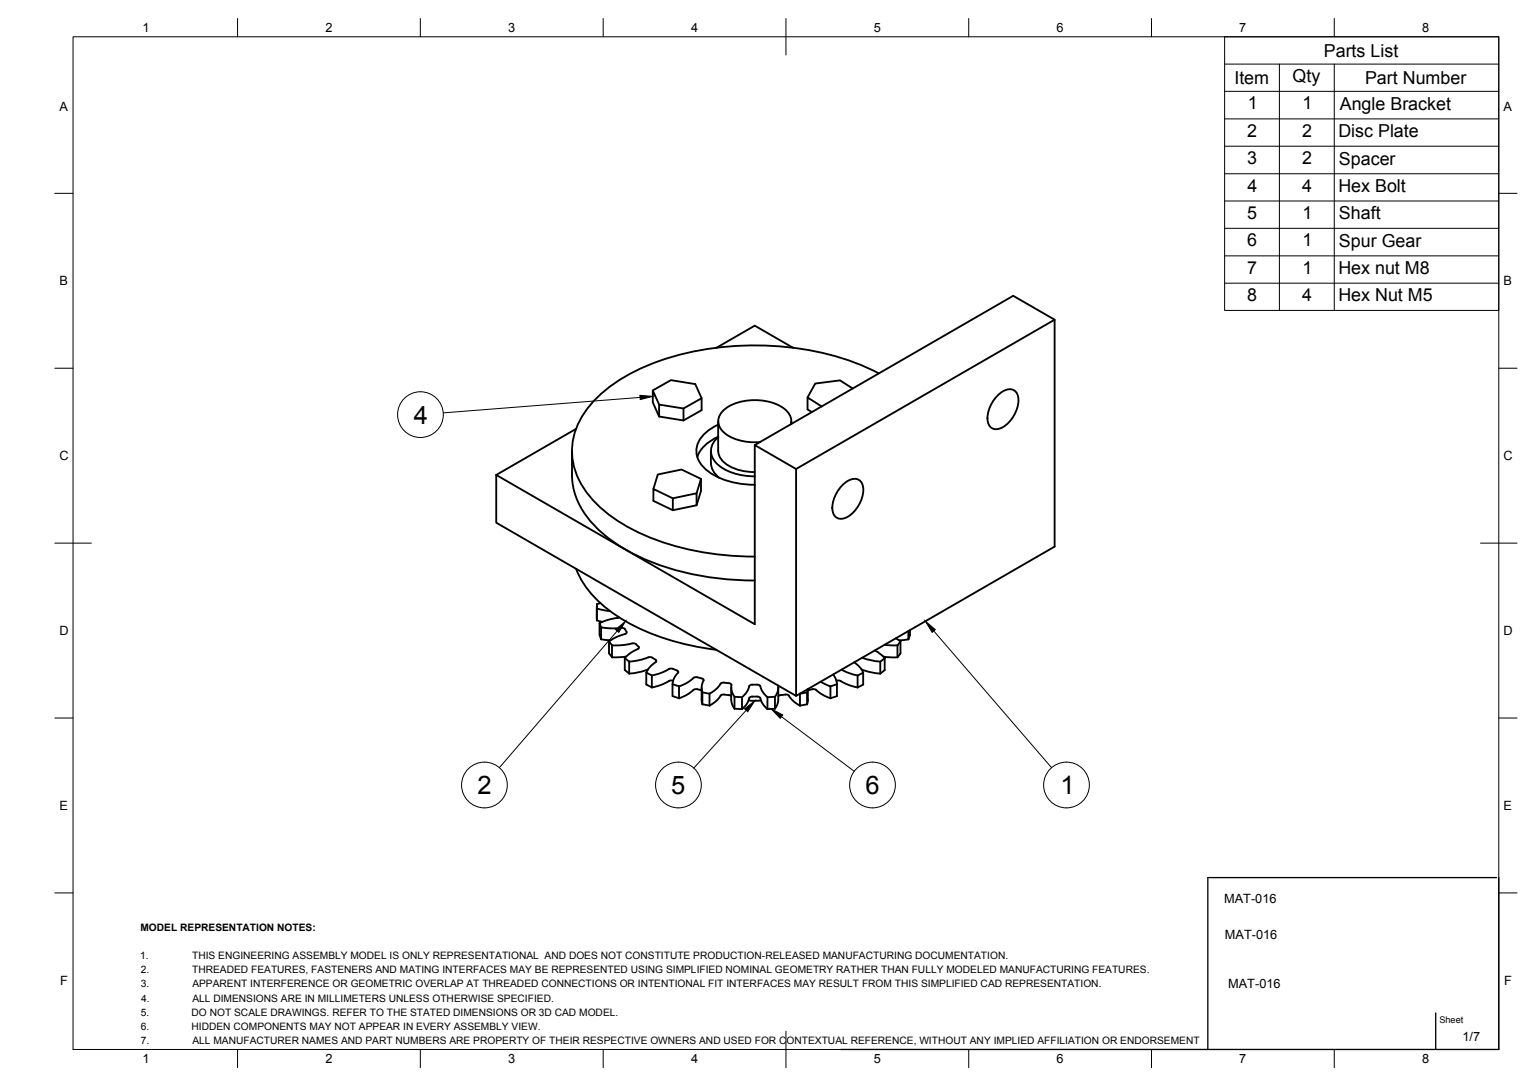
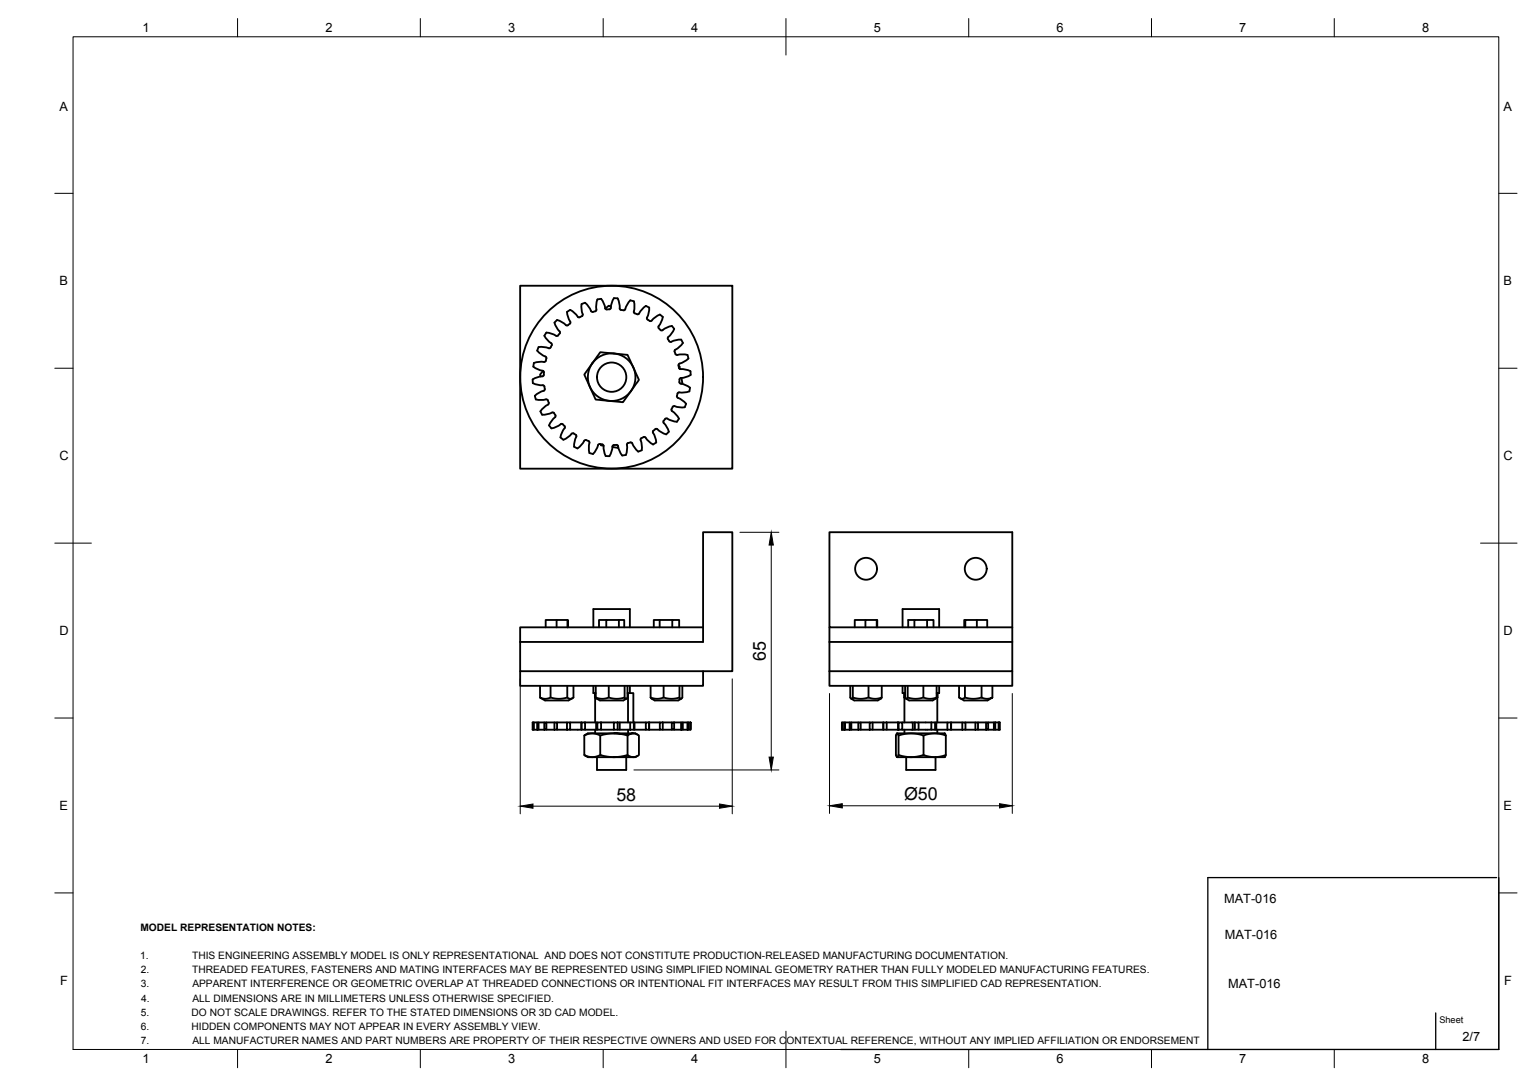
ISO-10303-21;
HEADER;
/* Generated by software containing ST-Developer
 * from STEP Tools, Inc. (www.steptools.com) 
 */

FILE_DESCRIPTION(
/* description */ ('STEP AP214'),
/* implementation_level */ '2;1');

FILE_NAME(
/* name */ 'MAT-016.step',
/* time_stamp */ '2026-11-14T06:10:26-08:00',
/* author */ (''),
/* organization */ (''),
/* preprocessor_version */ 'ST-DEVELOPER v20.2',
/* originating_system */ 'Autodesk Translation Framework v15.17.0.0',
/* authorisation */ '');

FILE_SCHEMA (('AUTOMOTIVE_DESIGN { 1 0 10303 214 3 1 1 }'));
ENDSEC;

DATA;
#10=MECHANICAL_DESIGN_GEOMETRIC_PRESENTATION_REPRESENTATION('',(#164,#165,
#166,#167,#168,#169,#170,#171),#10413);
#11=ITEM_DEFINED_TRANSFORMATION($,$,#5397,#6134);
#12=ITEM_DEFINED_TRANSFORMATION($,$,#6051,#6135);
#13=ITEM_DEFINED_TRANSFORMATION($,$,#6076,#6136);
#14=ITEM_DEFINED_TRANSFORMATION($,$,#6085,#6137);
#15=ITEM_DEFINED_TRANSFORMATION($,$,#5435,#6138);
#16=ITEM_DEFINED_TRANSFORMATION($,$,#5466,#6139);
#17=ITEM_DEFINED_TRANSFORMATION($,$,#6015,#6140);
#18=ITEM_DEFINED_TRANSFORMATION($,$,#6098,#6141);
#19=ITEM_DEFINED_TRANSFORMATION($,$,#6051,#6142);
#20=ITEM_DEFINED_TRANSFORMATION($,$,#6076,#6143);
#21=ITEM_DEFINED_TRANSFORMATION($,$,#6085,#6144);
#22=ITEM_DEFINED_TRANSFORMATION($,$,#6085,#6145);
#23=ITEM_DEFINED_TRANSFORMATION($,$,#6085,#6146);
#24=ITEM_DEFINED_TRANSFORMATION($,$,#6098,#6147);
#25=ITEM_DEFINED_TRANSFORMATION($,$,#6098,#6148);
#26=ITEM_DEFINED_TRANSFORMATION($,$,#6098,#6149);
#27=(
REPRESENTATION_RELATIONSHIP($,$,#10453,#10452)
REPRESENTATION_RELATIONSHIP_WITH_TRANSFORMATION(#11)
SHAPE_REPRESENTATION_RELATIONSHIP()
);
#28=(
REPRESENTATION_RELATIONSHIP($,$,#10457,#10452)
REPRESENTATION_RELATIONSHIP_WITH_TRANSFORMATION(#12)
SHAPE_REPRESENTATION_RELATIONSHIP()
);
#29=(
REPRESENTATION_RELATIONSHIP($,$,#10458,#10452)
REPRESENTATION_RELATIONSHIP_WITH_TRANSFORMATION(#13)
SHAPE_REPRESENTATION_RELATIONSHIP()
);
#30=(
REPRESENTATION_RELATIONSHIP($,$,#10459,#10452)
REPRESENTATION_RELATIONSHIP_WITH_TRANSFORMATION(#14)
SHAPE_REPRESENTATION_RELATIONSHIP()
);
#31=(
REPRESENTATION_RELATIONSHIP($,$,#10454,#10452)
REPRESENTATION_RELATIONSHIP_WITH_TRANSFORMATION(#15)
SHAPE_REPRESENTATION_RELATIONSHIP()
);
#32=(
REPRESENTATION_RELATIONSHIP($,$,#10455,#10452)
REPRESENTATION_RELATIONSHIP_WITH_TRANSFORMATION(#16)
SHAPE_REPRESENTATION_RELATIONSHIP()
);
#33=(
REPRESENTATION_RELATIONSHIP($,$,#10456,#10452)
REPRESENTATION_RELATIONSHIP_WITH_TRANSFORMATION(#17)
SHAPE_REPRESENTATION_RELATIONSHIP()
);
#34=(
REPRESENTATION_RELATIONSHIP($,$,#10460,#10452)
REPRESENTATION_RELATIONSHIP_WITH_TRANSFORMATION(#18)
SHAPE_REPRESENTATION_RELATIONSHIP()
);
#35=(
REPRESENTATION_RELATIONSHIP($,$,#10457,#10452)
REPRESENTATION_RELATIONSHIP_WITH_TRANSFORMATION(#19)
SHAPE_REPRESENTATION_RELATIONSHIP()
);
#36=(
REPRESENTATION_RELATIONSHIP($,$,#10458,#10452)
REPRESENTATION_RELATIONSHIP_WITH_TRANSFORMATION(#20)
SHAPE_REPRESENTATION_RELATIONSHIP()
);
#37=(
REPRESENTATION_RELATIONSHIP($,$,#10459,#10452)
REPRESENTATION_RELATIONSHIP_WITH_TRANSFORMATION(#21)
SHAPE_REPRESENTATION_RELATIONSHIP()
);
#38=(
REPRESENTATION_RELATIONSHIP($,$,#10459,#10452)
REPRESENTATION_RELATIONSHIP_WITH_TRANSFORMATION(#22)
SHAPE_REPRESENTATION_RELATIONSHIP()
);
#39=(
REPRESENTATION_RELATIONSHIP($,$,#10459,#10452)
REPRESENTATION_RELATIONSHIP_WITH_TRANSFORMATION(#23)
SHAPE_REPRESENTATION_RELATIONSHIP()
);
#40=(
REPRESENTATION_RELATIONSHIP($,$,#10460,#10452)
REPRESENTATION_RELATIONSHIP_WITH_TRANSFORMATION(#24)
SHAPE_REPRESENTATION_RELATIONSHIP()
);
#41=(
REPRESENTATION_RELATIONSHIP($,$,#10460,#10452)
REPRESENTATION_RELATIONSHIP_WITH_TRANSFORMATION(#25)
SHAPE_REPRESENTATION_RELATIONSHIP()
);
#42=(
REPRESENTATION_RELATIONSHIP($,$,#10460,#10452)
REPRESENTATION_RELATIONSHIP_WITH_TRANSFORMATION(#26)
SHAPE_REPRESENTATION_RELATIONSHIP()
);
#43=CONTEXT_DEPENDENT_SHAPE_REPRESENTATION(#27,#10436);
#44=CONTEXT_DEPENDENT_SHAPE_REPRESENTATION(#28,#10437);
#45=CONTEXT_DEPENDENT_SHAPE_REPRESENTATION(#29,#10438);
#46=CONTEXT_DEPENDENT_SHAPE_REPRESENTATION(#30,#10439);
#47=CONTEXT_DEPENDENT_SHAPE_REPRESENTATION(#31,#10440);
#48=CONTEXT_DEPENDENT_SHAPE_REPRESENTATION(#32,#10441);
#49=CONTEXT_DEPENDENT_SHAPE_REPRESENTATION(#33,#10442);
#50=CONTEXT_DEPENDENT_SHAPE_REPRESENTATION(#34,#10443);
#51=CONTEXT_DEPENDENT_SHAPE_REPRESENTATION(#35,#10444);
#52=CONTEXT_DEPENDENT_SHAPE_REPRESENTATION(#36,#10445);
#53=CONTEXT_DEPENDENT_SHAPE_REPRESENTATION(#37,#10446);
#54=CONTEXT_DEPENDENT_SHAPE_REPRESENTATION(#38,#10447);
#55=CONTEXT_DEPENDENT_SHAPE_REPRESENTATION(#39,#10448);
#56=CONTEXT_DEPENDENT_SHAPE_REPRESENTATION(#40,#10449);
#57=CONTEXT_DEPENDENT_SHAPE_REPRESENTATION(#41,#10450);
#58=CONTEXT_DEPENDENT_SHAPE_REPRESENTATION(#42,#10451);
#59=NEXT_ASSEMBLY_USAGE_OCCURRENCE('Angle Bracket:1','Angle Bracket:1',
'Angle Bracket:1',#10462,#10463,'Angle Bracket:1');
#60=NEXT_ASSEMBLY_USAGE_OCCURRENCE('Disc Plate:1','Disc Plate:1',
'Disc Plate:1',#10462,#10467,'Disc Plate:1');
#61=NEXT_ASSEMBLY_USAGE_OCCURRENCE('Spacer:1','Spacer:1','Spacer:1',#10462,
#10468,'Spacer:1');
#62=NEXT_ASSEMBLY_USAGE_OCCURRENCE('Hex Bolt:1','Hex Bolt:1',
'Hex Bolt:1',#10462,#10469,'Hex Bolt:1');
#63=NEXT_ASSEMBLY_USAGE_OCCURRENCE('Shaft:1','Shaft:1','Shaft:1',#10462,
#10464,'Shaft:1');
#64=NEXT_ASSEMBLY_USAGE_OCCURRENCE('Spur Gear:1','Spur Gear:1',
'Spur Gear:1',#10462,#10465,'Spur Gear:1');
#65=NEXT_ASSEMBLY_USAGE_OCCURRENCE('Hex Nut M8:1','Hex Nut M8:1',
'Hex Nut M8:1',#10462,#10466,'Hex Nut M8:1');
#66=NEXT_ASSEMBLY_USAGE_OCCURRENCE('Hex Nut M5:1','Hex Nut M5:1',
'Hex Nut M5:1',#10462,#10470,'Hex Nut M5:1');
#67=NEXT_ASSEMBLY_USAGE_OCCURRENCE('Disc Plate:2','Disc Plate:2',
'Disc Plate:2',#10462,#10467,'Disc Plate:2');
#68=NEXT_ASSEMBLY_USAGE_OCCURRENCE('Spacer:2','Spacer:2','Spacer:2',#10462,
#10468,'Spacer:2');
#69=NEXT_ASSEMBLY_USAGE_OCCURRENCE('Hex Bolt:2','Hex Bolt:2',
'Hex Bolt:2',#10462,#10469,'Hex Bolt:2');
#70=NEXT_ASSEMBLY_USAGE_OCCURRENCE('Hex Bolt:3','Hex Bolt:3',
'Hex Bolt:3',#10462,#10469,'Hex Bolt:3');
#71=NEXT_ASSEMBLY_USAGE_OCCURRENCE('Hex Bolt:4','Hex Bolt:4',
'Hex Bolt:4',#10462,#10469,'Hex Bolt:4');
#72=NEXT_ASSEMBLY_USAGE_OCCURRENCE('Hex Nut M5:2','Hex Nut M5:2',
'Hex Nut M5:2',#10462,#10470,'Hex Nut M5:2');
#73=NEXT_ASSEMBLY_USAGE_OCCURRENCE('Hex Nut M5:3','Hex Nut M5:3',
'Hex Nut M5:3',#10462,#10470,'Hex Nut M5:3');
#74=NEXT_ASSEMBLY_USAGE_OCCURRENCE('Hex Nut M5:4','Hex Nut M5:4',
'Hex Nut M5:4',#10462,#10470,'Hex Nut M5:4');
#75=(
BOUNDED_SURFACE()
B_SPLINE_SURFACE(1,2,((#10054,#10055,#10056,#10057,#10058,#10059,#10060,
#10061,#10062,#10063,#10064,#10065,#10066,#10067,#10068,#10069,#10070,#10071,
#10072,#10073,#10074,#10075,#10076,#10077,#10078,#10079,#10080,#10081,#10082,
#10083,#10084,#10085,#10086,#10087,#10088,#10089,#10090,#10091,#10092,#10093,
#10094,#10095,#10096,#10097,#10098,#10099,#10100,#10101,#10102,#10103,#10104,
#10105,#10106,#10107,#10108,#10109,#10110,#10111,#10112,#10113,#10114,#10115,
#10116,#10117,#10118,#10119,#10120,#10121,#10122,#10123,#10124,#10125,#10126,
#10127,#10128,#10129,#10130,#10131,#10132,#10133,#10134),(#10135,#10136,
#10137,#10138,#10139,#10140,#10141,#10142,#10143,#10144,#10145,#10146,#10147,
#10148,#10149,#10150,#10151,#10152,#10153,#10154,#10155,#10156,#10157,#10158,
#10159,#10160,#10161,#10162,#10163,#10164,#10165,#10166,#10167,#10168,#10169,
#10170,#10171,#10172,#10173,#10174,#10175,#10176,#10177,#10178,#10179,#10180,
#10181,#10182,#10183,#10184,#10185,#10186,#10187,#10188,#10189,#10190,#10191,
#10192,#10193,#10194,#10195,#10196,#10197,#10198,#10199,#10200,#10201,#10202,
#10203,#10204,#10205,#10206,#10207,#10208,#10209,#10210,#10211,#10212,#10213,
#10214,#10215)),.UNSPECIFIED.,.F.,.F.,.F.)
B_SPLINE_SURFACE_WITH_KNOTS((2,2),(3,2,2,2,2,2,2,2,2,2,2,2,2,2,2,2,2,2,
2,2,2,2,2,2,2,2,2,2,2,2,2,2,2,2,2,2,2,2,2,2,3),(-8.46272100971598E-5,1.),
(0.,0.025,0.05,0.075,0.1,0.125,0.15,0.175,0.2,0.225,0.25,0.275,0.3,0.325,
0.35,0.375,0.4,0.425,0.45,0.475,0.5,0.525,0.55,0.575,0.6,0.625,0.65,0.675,
0.7,0.725,0.75,0.775,0.8,0.825,0.85,0.875,0.9,0.925,0.95,0.975,1.),
 .UNSPECIFIED.)
GEOMETRIC_REPRESENTATION_ITEM()
RATIONAL_B_SPLINE_SURFACE(((1.,0.923879532511287,1.,0.923879532511287,1.,
0.923879532511287,1.,0.923879532511287,1.,0.923879532511287,1.,0.923879532511287,
1.,0.923879532511287,1.,0.923879532511287,1.,0.923879532511287,1.,0.923879532511287,
1.,0.923879532511287,1.,0.923879532511287,1.,0.923879532511287,1.,0.923879532511287,
1.,0.923879532511287,1.,0.923879532511287,1.,0.923879532511287,1.,0.923879532511287,
1.,0.923879532511287,1.,0.923879532511287,1.,0.923879532511287,1.,0.923879532511287,
1.,0.923879532511287,1.,0.923879532511287,1.,0.923879532511287,1.,0.923879532511287,
1.,0.923879532511287,1.,0.923879532511287,1.,0.923879532511287,1.,0.923879532511287,
1.,0.923879532511287,1.,0.923879532511287,1.,0.923879532511287,1.,0.923879532511287,
1.,0.923879532511287,1.,0.923879532511287,1.,0.923879532511287,1.,0.923879532511287,
1.,0.923879532511287,1.,0.923879532511287,1.),(1.,0.923879532511287,1.,
0.923879532511287,1.,0.923879532511287,1.,0.923879532511287,1.,0.923879532511287,
1.,0.923879532511287,1.,0.923879532511287,1.,0.923879532511287,1.,0.923879532511287,
1.,0.923879532511287,1.,0.923879532511287,1.,0.923879532511287,1.,0.923879532511287,
1.,0.923879532511287,1.,0.923879532511287,1.,0.923879532511287,1.,0.923879532511287,
1.,0.923879532511287,1.,0.923879532511287,1.,0.923879532511287,1.,0.923879532511287,
1.,0.923879532511287,1.,0.923879532511287,1.,0.923879532511287,1.,0.923879532511287,
1.,0.923879532511287,1.,0.923879532511287,1.,0.923879532511287,1.,0.923879532511287,
1.,0.923879532511287,1.,0.923879532511287,1.,0.923879532511287,1.,0.923879532511287,
1.,0.923879532511287,1.,0.923879532511287,1.,0.923879532511287,1.,0.923879532511287,
1.,0.923879532511287,1.,0.923879532511287,1.,0.923879532511287,1.)))
REPRESENTATION_ITEM('')
SURFACE()
);
#76=(
BOUNDED_SURFACE()
B_SPLINE_SURFACE(1,2,((#10216,#10217,#10218,#10219,#10220,#10221,#10222,
#10223,#10224,#10225,#10226,#10227,#10228,#10229,#10230,#10231,#10232,#10233,
#10234,#10235,#10236,#10237,#10238,#10239,#10240,#10241,#10242,#10243,#10244,
#10245,#10246,#10247,#10248,#10249,#10250,#10251,#10252,#10253,#10254,#10255,
#10256,#10257,#10258,#10259,#10260,#10261,#10262,#10263,#10264,#10265,#10266,
#10267,#10268,#10269,#10270,#10271,#10272,#10273,#10274,#10275,#10276,#10277,
#10278,#10279,#10280,#10281,#10282,#10283,#10284,#10285,#10286,#10287,#10288,
#10289,#10290,#10291,#10292,#10293,#10294,#10295,#10296),(#10297,#10298,
#10299,#10300,#10301,#10302,#10303,#10304,#10305,#10306,#10307,#10308,#10309,
#10310,#10311,#10312,#10313,#10314,#10315,#10316,#10317,#10318,#10319,#10320,
#10321,#10322,#10323,#10324,#10325,#10326,#10327,#10328,#10329,#10330,#10331,
#10332,#10333,#10334,#10335,#10336,#10337,#10338,#10339,#10340,#10341,#10342,
#10343,#10344,#10345,#10346,#10347,#10348,#10349,#10350,#10351,#10352,#10353,
#10354,#10355,#10356,#10357,#10358,#10359,#10360,#10361,#10362,#10363,#10364,
#10365,#10366,#10367,#10368,#10369,#10370,#10371,#10372,#10373,#10374,#10375,
#10376,#10377)),.UNSPECIFIED.,.F.,.F.,.F.)
B_SPLINE_SURFACE_WITH_KNOTS((2,2),(3,2,2,2,2,2,2,2,2,2,2,2,2,2,2,2,2,2,
2,2,2,2,2,2,2,2,2,2,2,2,2,2,2,2,2,2,2,2,2,2,3),(0.,1.00002043531825),(0.,
0.025,0.05,0.075,0.1,0.125,0.15,0.175,0.2,0.225,0.25,0.275,0.3,0.325,0.35,
0.375,0.4,0.425,0.45,0.475,0.5,0.525,0.55,0.575,0.6,0.625,0.65,0.675,0.7,
0.725,0.75,0.775,0.8,0.825,0.85,0.875,0.9,0.925,0.95,0.975,1.),
 .UNSPECIFIED.)
GEOMETRIC_REPRESENTATION_ITEM()
RATIONAL_B_SPLINE_SURFACE(((1.,0.923879532511287,1.,0.923879532511287,1.,
0.923879532511287,1.,0.923879532511287,1.,0.923879532511287,1.,0.923879532511287,
1.,0.923879532511287,1.,0.923879532511287,1.,0.923879532511287,1.,0.923879532511287,
1.,0.923879532511287,1.,0.923879532511287,1.,0.923879532511287,1.,0.923879532511287,
1.,0.923879532511287,1.,0.923879532511287,1.,0.923879532511287,1.,0.923879532511287,
1.,0.923879532511287,1.,0.923879532511287,1.,0.923879532511287,1.,0.923879532511287,
1.,0.923879532511287,1.,0.923879532511287,1.,0.923879532511287,1.,0.923879532511287,
1.,0.923879532511287,1.,0.923879532511287,1.,0.923879532511287,1.,0.923879532511287,
1.,0.923879532511287,1.,0.923879532511287,1.,0.923879532511287,1.,0.923879532511287,
1.,0.923879532511287,1.,0.923879532511287,1.,0.923879532511287,1.,0.923879532511287,
1.,0.923879532511287,1.,0.923879532511287,1.),(1.,0.923879532511287,1.,
0.923879532511287,1.,0.923879532511287,1.,0.923879532511287,1.,0.923879532511287,
1.,0.923879532511287,1.,0.923879532511287,1.,0.923879532511287,1.,0.923879532511287,
1.,0.923879532511287,1.,0.923879532511287,1.,0.923879532511287,1.,0.923879532511287,
1.,0.923879532511287,1.,0.923879532511287,1.,0.923879532511287,1.,0.923879532511287,
1.,0.923879532511287,1.,0.923879532511287,1.,0.923879532511287,1.,0.923879532511287,
1.,0.923879532511287,1.,0.923879532511287,1.,0.923879532511287,1.,0.923879532511287,
1.,0.923879532511287,1.,0.923879532511287,1.,0.923879532511287,1.,0.923879532511287,
1.,0.923879532511287,1.,0.923879532511287,1.,0.923879532511287,1.,0.923879532511287,
1.,0.923879532511287,1.,0.923879532511287,1.,0.923879532511287,1.,0.923879532511287,
1.,0.923879532511287,1.,0.923879532511287,1.,0.923879532511287,1.)))
REPRESENTATION_ITEM('')
SURFACE()
);
#77=B_SPLINE_CURVE_WITH_KNOTS('',3,(#9606,#9607,#9608,#9609,#9610,#9611,
#9612,#9613,#9614,#9615,#9616,#9617),.UNSPECIFIED.,.F.,.F.,(4,2,2,2,2,4),
(0.,0.0440198106719265,0.0818393800786219,0.0973901488912384,0.118004089223957,
0.138865194736436),.UNSPECIFIED.);
#78=B_SPLINE_CURVE_WITH_KNOTS('',3,(#9624,#9625,#9626,#9627,#9628,#9629,
#9630,#9631,#9632,#9633,#9634,#9635,#9636,#9637),.UNSPECIFIED.,.F.,.F.,
(4,2,2,2,2,2,4),(0.65296058419034,0.667191402073545,0.721861714124772,0.750052142288269,
0.80044940087167,0.822940957368803,0.845554952657274),.UNSPECIFIED.);
#79=B_SPLINE_CURVE_WITH_KNOTS('',3,(#9641,#9642,#9643,#9644,#9645,#9646,
#9647,#9648,#9649,#9650),.UNSPECIFIED.,.F.,.F.,(4,2,2,2,4),(0.,0.0725503805935694,
0.183171338078937,0.39459654609614,0.611301898072818),.UNSPECIFIED.);
#80=B_SPLINE_CURVE_WITH_KNOTS('',3,(#9656,#9657,#9658,#9659,#9660,#9661,
#9662,#9663,#9664,#9665,#9666,#9667,#9668,#9669,#9670,#9671,#9672,#9673,
#9674,#9675,#9676,#9677,#9678,#9679,#9680,#9681,#9682,#9683),
 .UNSPECIFIED.,.F.,.F.,(4,2,2,2,2,2,2,2,2,2,2,2,2,4),(2.8604222096497,2.92399815097309,
3.00151852083596,3.07984339341042,3.15735934738356,3.23558227378115,3.31309753786526,
3.39121939156188,3.46873767665382,3.54675946426518,3.62428444893176,3.70220732091536,
3.75130237269173,3.79952779459516),.UNSPECIFIED.);
#81=B_SPLINE_CURVE_WITH_KNOTS('',3,(#9684,#9685,#9686,#9687,#9688,#9689,
#9690,#9691,#9692,#9693,#9694,#9695,#9696,#9697,#9698,#9699,#9700,#9701,
#9702,#9703,#9704,#9705,#9706,#9707,#9708,#9709,#9710,#9711,#9712,#9713,
#9714,#9715,#9716,#9717,#9718,#9719),.UNSPECIFIED.,.F.,.F.,(4,2,2,2,2,2,
2,2,2,2,2,2,2,2,2,2,2,4),(9.99999999976564E-7,0.0723571430117073,0.145111301826658,
0.22257528520235,0.302853983952927,0.38026926760894,0.460477482838669,0.537847198345145,
0.617986080669744,0.695313511929628,0.775384190116896,0.852672774273399,
0.932676349504524,1.00992967673158,1.08986721715565,1.16708902919314,1.24696156497064,
1.26600100077784),.UNSPECIFIED.);
#82=B_SPLINE_CURVE_WITH_KNOTS('',3,(#9724,#9725,#9726,#9727,#9728,#9729,
#9730,#9731,#9732,#9733,#9734,#9735,#9736,#9737,#9738,#9739,#9740,#9741,
#9742,#9743,#9744,#9745,#9746,#9747,#9748,#9749,#9750,#9751,#9752,#9753,
#9754,#9755,#9756,#9757,#9758,#9759),.UNSPECIFIED.,.F.,.F.,(4,2,2,2,2,2,
2,2,2,2,2,2,2,2,2,2,2,4),(1.60361927798793,1.67068837178043,1.75059716351924,
1.82756418592221,1.90739668701968,1.98645074137197,2.06407483714533,2.14302368536841,
2.22062153982352,2.29946541005855,2.37704053193709,2.45577971634894,2.53333568134052,
2.61197054470874,2.68951098486698,2.76804197371372,2.84557056555073,2.8604222096497),
 .UNSPECIFIED.);
#83=B_SPLINE_CURVE_WITH_KNOTS('',3,(#9760,#9761,#9762,#9763,#9764,#9765,
#9766,#9767,#9768,#9769,#9770,#9771,#9772,#9773,#9774,#9775,#9776,#9777,
#9778,#9779,#9780,#9781,#9782,#9783,#9784,#9785,#9786,#9787,#9788,#9789,
#9790,#9791,#9792,#9793,#9794,#9795),.UNSPECIFIED.,.F.,.F.,(4,2,2,2,2,2,
2,2,2,2,2,2,2,2,2,2,2,4),(1.26600100077784,1.32415579820781,1.40396438029636,
1.48113503862289,1.56088054628166,1.63803178784153,1.71771511568453,1.79485124435928,
1.87447323848536,1.95159867942297,2.03003619734553,2.1081949238022,2.18666282399953,
2.26473464872532,2.34323576121314,2.42122333365511,2.49976031435316,2.52861029293173),
 .UNSPECIFIED.);
#84=B_SPLINE_CURVE_WITH_KNOTS('',3,(#9800,#9801,#9802,#9803),
 .UNSPECIFIED.,.F.,.F.,(4,4),(3.78986857128077,3.8120765287242),
 .UNSPECIFIED.);
#85=B_SPLINE_CURVE_WITH_KNOTS('',3,(#9804,#9805,#9806,#9807,#9808,#9809,
#9810,#9811,#9812,#9813,#9814,#9815,#9816,#9817),.UNSPECIFIED.,.F.,.F.,
(4,2,2,2,2,2,4),(9.99999999715276E-7,0.046357433654922,0.0937119022879353,
0.174442583515723,0.25212318836089,0.332767216413102,0.339556120788476),
 .UNSPECIFIED.);
#86=B_SPLINE_CURVE_WITH_KNOTS('',3,(#9819,#9820,#9821,#9822,#9823,#9824,
#9825,#9826,#9827,#9828,#9829,#9830,#9831,#9832,#9833,#9834,#9835,#9836,
#9837,#9838,#9839,#9840,#9841,#9842,#9843,#9844,#9845,#9846,#9847,#9848,
#9849,#9850,#9851,#9852,#9853,#9854),.UNSPECIFIED.,.F.,.F.,(4,2,2,2,2,2,
2,2,2,2,2,2,2,2,2,2,2,4),(0.339556120788476,0.41036939162952,0.490927908821085,
0.568452828064013,0.648926534411366,0.726375625006592,0.806765489869361,
0.884140289007795,0.964447312664774,1.04174945254203,1.12197466490902,1.1992058779733,
1.27935033693266,1.35651246121441,1.43657725052838,1.5136722350114,1.5936584617954,
1.60361927798793),.UNSPECIFIED.);
#87=B_SPLINE_CURVE_WITH_KNOTS('',3,(#9855,#9856,#9857,#9858,#9859,#9860,
#9861,#9862,#9863,#9864,#9865,#9866,#9867,#9868,#9869,#9870,#9871,#9872,
#9873,#9874,#9875,#9876,#9877,#9878,#9879,#9880,#9881,#9882,#9883,#9884,
#9885,#9886,#9887,#9888,#9889,#9890),.UNSPECIFIED.,.F.,.F.,(4,2,2,2,2,2,
2,2,2,2,2,2,2,2,2,2,2,4),(2.52861029293173,2.57766649346594,2.65624181672742,
2.73406967065805,2.8126856246171,2.89043842827534,2.9690971131827,3.0467783436143,
3.12548167324701,3.20309500277339,3.28184470891144,3.359393996049,3.43819163591573,
3.51568091413997,3.5945278806067,3.67196134507875,3.74273037840176,3.78986857128077),
 .UNSPECIFIED.);
#88=B_SPLINE_CURVE_WITH_KNOTS('',3,(#9926,#9927,#9928,#9929,#9930,#9931,
#9932,#9933,#9934,#9935,#9936,#9937,#9938,#9939,#9940,#9941,#9942,#9943,
#9944,#9945,#9946,#9947,#9948,#9949,#9950,#9951),.UNSPECIFIED.,.F.,.F.,
(4,2,2,2,2,2,2,2,2,2,2,2,4),(1.00000005114759E-6,0.0504044288517504,0.101697907474949,
0.196791682582806,0.281186634272934,0.358208836397077,0.426888278521547,
0.487555064818087,0.518648689337668,0.549949053437167,0.607608841009272,
0.637237664676633,0.65296058419034),.UNSPECIFIED.);
#89=B_SPLINE_CURVE_WITH_KNOTS('',3,(#9955,#9956,#9957,#9958,#9959,#9960,
#9961,#9962,#9963,#9964,#9965,#9966,#9967,#9968,#9969,#9970,#9971,#9972,
#9973,#9974,#9975,#9976,#9977,#9978,#9979,#9980,#9981,#9982,#9983,#9984,
#9985,#9986,#9987,#9988),.UNSPECIFIED.,.F.,.F.,(4,2,2,2,2,2,2,2,2,2,2,2,
2,2,2,2,4),(-0.463997948906847,-0.451682823252161,-0.441542190454548,-0.42099125853003,
-0.408322861738078,-0.395698404917208,-0.371037580166826,-0.34212985279081,
-0.311147419702825,-0.294752355985258,-0.261382300325676,-0.244928786327198,
-0.207389215554967,-0.164348973242395,-0.11566569854488,-0.0657340977400675,
-9.99999999292063E-7),.UNSPECIFIED.);
#90=(
BOUNDED_CURVE()
B_SPLINE_CURVE(2,(#9232,#9233,#9234),.UNSPECIFIED.,.F.,.F.)
B_SPLINE_CURVE_WITH_KNOTS((3,3),(-2.73681737299457,-1.98462831214807),
 .UNSPECIFIED.)
CURVE()
GEOMETRIC_REPRESENTATION_ITEM()
RATIONAL_B_SPLINE_CURVE((1.85571966561192,1.99926008128974,1.99926008128974))
REPRESENTATION_ITEM('')
);
#91=(
BOUNDED_CURVE()
B_SPLINE_CURVE(2,(#9235,#9236,#9237),.UNSPECIFIED.,.F.,.F.)
B_SPLINE_CURVE_WITH_KNOTS((3,3),(1.98462831214807,2.73681737299457),
 .UNSPECIFIED.)
CURVE()
GEOMETRIC_REPRESENTATION_ITEM()
RATIONAL_B_SPLINE_CURVE((1.99926008128974,1.99926008128974,1.85571966561192))
REPRESENTATION_ITEM('')
);
#92=(
BOUNDED_CURVE()
B_SPLINE_CURVE(2,(#9243,#9244,#9245),.UNSPECIFIED.,.F.,.F.)
B_SPLINE_CURVE_WITH_KNOTS((3,3),(1.98462831214807,2.73681737299457),
 .UNSPECIFIED.)
CURVE()
GEOMETRIC_REPRESENTATION_ITEM()
RATIONAL_B_SPLINE_CURVE((1.99926008128974,1.99926008128974,1.85571966561192))
REPRESENTATION_ITEM('')
);
#93=(
BOUNDED_CURVE()
B_SPLINE_CURVE(2,(#9246,#9247,#9248),.UNSPECIFIED.,.F.,.F.)
B_SPLINE_CURVE_WITH_KNOTS((3,3),(-2.73681737299457,-1.98462831214807),
 .UNSPECIFIED.)
CURVE()
GEOMETRIC_REPRESENTATION_ITEM()
RATIONAL_B_SPLINE_CURVE((1.85571966561192,1.99926008128974,1.99926008128974))
REPRESENTATION_ITEM('')
);
#94=(
BOUNDED_CURVE()
B_SPLINE_CURVE(2,(#9252,#9253,#9254),.UNSPECIFIED.,.F.,.F.)
B_SPLINE_CURVE_WITH_KNOTS((3,3),(-1.98462831214807,-1.23243925130156),
 .UNSPECIFIED.)
CURVE()
GEOMETRIC_REPRESENTATION_ITEM()
RATIONAL_B_SPLINE_CURVE((1.99926008128974,1.99926008128975,1.85571966561192))
REPRESENTATION_ITEM('')
);
#95=(
BOUNDED_CURVE()
B_SPLINE_CURVE(2,(#9257,#9258,#9259),.UNSPECIFIED.,.F.,.F.)
B_SPLINE_CURVE_WITH_KNOTS((3,3),(1.98462831214807,2.73681737299457),
 .UNSPECIFIED.)
CURVE()
GEOMETRIC_REPRESENTATION_ITEM()
RATIONAL_B_SPLINE_CURVE((1.99926008128974,1.99926008128974,1.85571966561192))
REPRESENTATION_ITEM('')
);
#96=(
BOUNDED_CURVE()
B_SPLINE_CURVE(2,(#9264,#9265,#9266),.UNSPECIFIED.,.F.,.F.)
B_SPLINE_CURVE_WITH_KNOTS((3,3),(-2.73681737299457,-1.98462831214807),
 .UNSPECIFIED.)
CURVE()
GEOMETRIC_REPRESENTATION_ITEM()
RATIONAL_B_SPLINE_CURVE((1.85571966561192,1.99926008128974,1.99926008128974))
REPRESENTATION_ITEM('')
);
#97=(
BOUNDED_CURVE()
B_SPLINE_CURVE(2,(#9267,#9268,#9269),.UNSPECIFIED.,.F.,.F.)
B_SPLINE_CURVE_WITH_KNOTS((3,3),(1.23243925130156,1.98462831214807),
 .UNSPECIFIED.)
CURVE()
GEOMETRIC_REPRESENTATION_ITEM()
RATIONAL_B_SPLINE_CURVE((1.85571966561192,1.99926008128974,1.99926008128974))
REPRESENTATION_ITEM('')
);
#98=(
BOUNDED_CURVE()
B_SPLINE_CURVE(2,(#9275,#9276,#9277),.UNSPECIFIED.,.F.,.F.)
B_SPLINE_CURVE_WITH_KNOTS((3,3),(-2.73681737299457,-1.98462831214806),
 .UNSPECIFIED.)
CURVE()
GEOMETRIC_REPRESENTATION_ITEM()
RATIONAL_B_SPLINE_CURVE((1.85571966561192,1.99926008128974,1.99926008128974))
REPRESENTATION_ITEM('')
);
#99=(
BOUNDED_CURVE()
B_SPLINE_CURVE(2,(#9278,#9279,#9280),.UNSPECIFIED.,.F.,.F.)
B_SPLINE_CURVE_WITH_KNOTS((3,3),(-1.98462831214806,-1.23243925130156),
 .UNSPECIFIED.)
CURVE()
GEOMETRIC_REPRESENTATION_ITEM()
RATIONAL_B_SPLINE_CURVE((1.99926008128974,1.99926008128974,1.85571966561192))
REPRESENTATION_ITEM('')
);
#100=(
BOUNDED_CURVE()
B_SPLINE_CURVE(2,(#9282,#9283,#9284),.UNSPECIFIED.,.F.,.F.)
B_SPLINE_CURVE_WITH_KNOTS((3,3),(1.98462831214807,2.73681737299457),
 .UNSPECIFIED.)
CURVE()
GEOMETRIC_REPRESENTATION_ITEM()
RATIONAL_B_SPLINE_CURVE((1.99926008128974,1.99926008128974,1.85571966561192))
REPRESENTATION_ITEM('')
);
#101=(
BOUNDED_CURVE()
B_SPLINE_CURVE(2,(#9285,#9286,#9287),.UNSPECIFIED.,.F.,.F.)
B_SPLINE_CURVE_WITH_KNOTS((3,3),(1.23243925130156,1.98462831214807),
 .UNSPECIFIED.)
CURVE()
GEOMETRIC_REPRESENTATION_ITEM()
RATIONAL_B_SPLINE_CURVE((1.85571966561192,1.99926008128974,1.99926008128974))
REPRESENTATION_ITEM('')
);
#102=(
BOUNDED_CURVE()
B_SPLINE_CURVE(2,(#9293,#9294,#9295),.UNSPECIFIED.,.F.,.F.)
B_SPLINE_CURVE_WITH_KNOTS((3,3),(-2.73681737299457,-1.98462831214807),
 .UNSPECIFIED.)
CURVE()
GEOMETRIC_REPRESENTATION_ITEM()
RATIONAL_B_SPLINE_CURVE((1.85571966561192,1.99926008128974,1.99926008128974))
REPRESENTATION_ITEM('')
);
#103=(
BOUNDED_CURVE()
B_SPLINE_CURVE(2,(#9296,#9297,#9298),.UNSPECIFIED.,.F.,.F.)
B_SPLINE_CURVE_WITH_KNOTS((3,3),(-1.98462831214807,-1.23243925130157),
 .UNSPECIFIED.)
CURVE()
GEOMETRIC_REPRESENTATION_ITEM()
RATIONAL_B_SPLINE_CURVE((1.99926008128974,1.99926008128974,1.85571966561192))
REPRESENTATION_ITEM('')
);
#104=(
BOUNDED_CURVE()
B_SPLINE_CURVE(2,(#9300,#9301,#9302),.UNSPECIFIED.,.F.,.F.)
B_SPLINE_CURVE_WITH_KNOTS((3,3),(1.98462831214807,2.73681737299457),
 .UNSPECIFIED.)
CURVE()
GEOMETRIC_REPRESENTATION_ITEM()
RATIONAL_B_SPLINE_CURVE((1.99926008128974,1.99926008128974,1.85571966561192))
REPRESENTATION_ITEM('')
);
#105=(
BOUNDED_CURVE()
B_SPLINE_CURVE(2,(#9303,#9304,#9305),.UNSPECIFIED.,.F.,.F.)
B_SPLINE_CURVE_WITH_KNOTS((3,3),(1.23243925130156,1.98462831214807),
 .UNSPECIFIED.)
CURVE()
GEOMETRIC_REPRESENTATION_ITEM()
RATIONAL_B_SPLINE_CURVE((1.85571966561192,1.99926008128974,1.99926008128974))
REPRESENTATION_ITEM('')
);
#106=(
BOUNDED_CURVE()
B_SPLINE_CURVE(2,(#9311,#9312,#9313),.UNSPECIFIED.,.F.,.F.)
B_SPLINE_CURVE_WITH_KNOTS((3,3),(-2.73681737299457,-1.98462831214807),
 .UNSPECIFIED.)
CURVE()
GEOMETRIC_REPRESENTATION_ITEM()
RATIONAL_B_SPLINE_CURVE((1.85571966561192,1.99926008128974,1.99926008128974))
REPRESENTATION_ITEM('')
);
#107=(
BOUNDED_CURVE()
B_SPLINE_CURVE(2,(#9314,#9315,#9316),.UNSPECIFIED.,.F.,.F.)
B_SPLINE_CURVE_WITH_KNOTS((3,3),(-1.98462831214807,-1.23243925130157),
 .UNSPECIFIED.)
CURVE()
GEOMETRIC_REPRESENTATION_ITEM()
RATIONAL_B_SPLINE_CURVE((1.99926008128974,1.99926008128974,1.85571966561192))
REPRESENTATION_ITEM('')
);
#108=(
BOUNDED_CURVE()
B_SPLINE_CURVE(2,(#9318,#9319,#9320),.UNSPECIFIED.,.F.,.F.)
B_SPLINE_CURVE_WITH_KNOTS((3,3),(1.98462831214807,2.73681737299457),
 .UNSPECIFIED.)
CURVE()
GEOMETRIC_REPRESENTATION_ITEM()
RATIONAL_B_SPLINE_CURVE((1.99926008128974,1.99926008128974,1.85571966561192))
REPRESENTATION_ITEM('')
);
#109=(
BOUNDED_CURVE()
B_SPLINE_CURVE(2,(#9321,#9322,#9323),.UNSPECIFIED.,.F.,.F.)
B_SPLINE_CURVE_WITH_KNOTS((3,3),(1.23243925130157,1.98462831214807),
 .UNSPECIFIED.)
CURVE()
GEOMETRIC_REPRESENTATION_ITEM()
RATIONAL_B_SPLINE_CURVE((1.85571966561192,1.99926008128974,1.99926008128974))
REPRESENTATION_ITEM('')
);
#110=(
BOUNDED_CURVE()
B_SPLINE_CURVE(2,(#9326,#9327,#9328),.UNSPECIFIED.,.F.,.F.)
B_SPLINE_CURVE_WITH_KNOTS((3,3),(-2.73681737299457,-1.98462831214806),
 .UNSPECIFIED.)
CURVE()
GEOMETRIC_REPRESENTATION_ITEM()
RATIONAL_B_SPLINE_CURVE((1.85571966561192,1.99926008128974,1.99926008128974))
REPRESENTATION_ITEM('')
);
#111=(
BOUNDED_CURVE()
B_SPLINE_CURVE(2,(#9329,#9330,#9331),.UNSPECIFIED.,.F.,.F.)
B_SPLINE_CURVE_WITH_KNOTS((3,3),(-1.98462831214806,-1.23243925130156),
 .UNSPECIFIED.)
CURVE()
GEOMETRIC_REPRESENTATION_ITEM()
RATIONAL_B_SPLINE_CURVE((1.99926008128974,1.99926008128974,1.85571966561192))
REPRESENTATION_ITEM('')
);
#112=(
BOUNDED_CURVE()
B_SPLINE_CURVE(2,(#9333,#9334,#9335),.UNSPECIFIED.,.F.,.F.)
B_SPLINE_CURVE_WITH_KNOTS((3,3),(1.98462831214807,2.73681737299457),
 .UNSPECIFIED.)
CURVE()
GEOMETRIC_REPRESENTATION_ITEM()
RATIONAL_B_SPLINE_CURVE((1.99926008128974,1.99926008128974,1.85571966561191))
REPRESENTATION_ITEM('')
);
#113=(
BOUNDED_CURVE()
B_SPLINE_CURVE(2,(#9336,#9337,#9338),.UNSPECIFIED.,.F.,.F.)
B_SPLINE_CURVE_WITH_KNOTS((3,3),(1.23243925130156,1.98462831214807),
 .UNSPECIFIED.)
CURVE()
GEOMETRIC_REPRESENTATION_ITEM()
RATIONAL_B_SPLINE_CURVE((1.85571966561192,1.99926008128974,1.99926008128974))
REPRESENTATION_ITEM('')
);
#114=(
BOUNDED_CURVE()
B_SPLINE_CURVE(2,(#9474,#9475,#9476,#9477,#9478,#9479,#9480,#9481,#9482,
#9483,#9484),.UNSPECIFIED.,.F.,.F.)
B_SPLINE_CURVE_WITH_KNOTS((3,2,2,2,2,3),(0.7,0.725,0.75,0.775,0.8,0.814142575738201),
 .UNSPECIFIED.)
CURVE()
GEOMETRIC_REPRESENTATION_ITEM()
RATIONAL_B_SPLINE_CURVE((1.,0.923879532511287,1.,0.923879532511287,1.,0.923879532511287,
1.,0.923879532511287,1.,0.956938420932543,0.962596973334531))
REPRESENTATION_ITEM('')
);
#115=(
BOUNDED_CURVE()
B_SPLINE_CURVE(2,(#9487,#9488,#9489,#9490,#9491,#9492,#9493,#9494,#9495,
#9496,#9497,#9498,#9499),.UNSPECIFIED.,.F.,.F.)
B_SPLINE_CURVE_WITH_KNOTS((3,2,2,2,2,2,3),(0.7,0.725,0.75,0.775,0.8,0.825,
0.839142575738204),.UNSPECIFIED.)
CURVE()
GEOMETRIC_REPRESENTATION_ITEM()
RATIONAL_B_SPLINE_CURVE((1.,0.923879532511287,1.,0.923879532511287,1.,0.923879532511287,
1.,0.923879532511287,1.,0.923879532511287,1.,0.956938420932534,0.962596973334533))
REPRESENTATION_ITEM('')
);
#116=(
BOUNDED_CURVE()
B_SPLINE_CURVE(2,(#9504,#9505,#9506,#9507,#9508,#9509,#9510,#9511,#9512,
#9513,#9514,#9515,#9516,#9517,#9518,#9519,#9520),.UNSPECIFIED.,.F.,.F.)
B_SPLINE_CURVE_WITH_KNOTS((3,2,2,2,2,2,2,2,3),(0.5,0.525,0.55,0.575,0.6,
0.625,0.65,0.675,0.7),.UNSPECIFIED.)
CURVE()
GEOMETRIC_REPRESENTATION_ITEM()
RATIONAL_B_SPLINE_CURVE((1.,0.923879532511287,1.,0.923879532511287,1.,0.923879532511287,
1.,0.923879532511287,1.,0.923879532511287,1.,0.923879532511287,1.,0.923879532511287,
1.,0.923879532511287,1.))
REPRESENTATION_ITEM('')
);
#117=(
BOUNDED_CURVE()
B_SPLINE_CURVE(2,(#9521,#9522,#9523,#9524,#9525,#9526,#9527,#9528,#9529,
#9530,#9531,#9532,#9533,#9534,#9535,#9536,#9537),.UNSPECIFIED.,.F.,.F.)
B_SPLINE_CURVE_WITH_KNOTS((3,2,2,2,2,2,2,2,3),(0.5,0.525,0.55,0.575,0.6,
0.625,0.65,0.675,0.7),.UNSPECIFIED.)
CURVE()
GEOMETRIC_REPRESENTATION_ITEM()
RATIONAL_B_SPLINE_CURVE((1.,0.923879532511287,1.,0.923879532511287,1.,0.923879532511287,
1.,0.923879532511287,1.,0.923879532511287,1.,0.923879532511287,1.,0.923879532511287,
1.,0.923879532511287,1.))
REPRESENTATION_ITEM('')
);
#118=(
BOUNDED_CURVE()
B_SPLINE_CURVE(2,(#9542,#9543,#9544,#9545,#9546,#9547,#9548,#9549,#9550,
#9551,#9552,#9553,#9554,#9555,#9556,#9557,#9558),.UNSPECIFIED.,.F.,.F.)
B_SPLINE_CURVE_WITH_KNOTS((3,2,2,2,2,2,2,2,3),(0.3,0.325,0.35,0.375,0.4,
0.425,0.45,0.475,0.5),.UNSPECIFIED.)
CURVE()
GEOMETRIC_REPRESENTATION_ITEM()
RATIONAL_B_SPLINE_CURVE((1.,0.923879532511287,1.,0.923879532511287,1.,0.923879532511287,
1.,0.923879532511287,1.,0.923879532511287,1.,0.923879532511287,1.,0.923879532511287,
1.,0.923879532511287,1.))
REPRESENTATION_ITEM('')
);
#119=(
BOUNDED_CURVE()
B_SPLINE_CURVE(2,(#9559,#9560,#9561,#9562,#9563,#9564,#9565,#9566,#9567,
#9568,#9569,#9570,#9571,#9572,#9573,#9574,#9575),.UNSPECIFIED.,.F.,.F.)
B_SPLINE_CURVE_WITH_KNOTS((3,2,2,2,2,2,2,2,3),(0.3,0.325,0.35,0.375,0.4,
0.425,0.45,0.475,0.5),.UNSPECIFIED.)
CURVE()
GEOMETRIC_REPRESENTATION_ITEM()
RATIONAL_B_SPLINE_CURVE((1.,0.923879532511287,1.,0.923879532511287,1.,0.923879532511287,
1.,0.923879532511287,1.,0.923879532511287,1.,0.923879532511287,1.,0.923879532511287,
1.,0.923879532511287,1.))
REPRESENTATION_ITEM('')
);
#120=(
BOUNDED_CURVE()
B_SPLINE_CURVE(2,(#9581,#9582,#9583,#9584,#9585,#9586,#9587),
 .UNSPECIFIED.,.F.,.F.)
B_SPLINE_CURVE_WITH_KNOTS((3,2,2,3),(0.0391425757382012,0.05,0.075,0.1),
 .UNSPECIFIED.)
CURVE()
GEOMETRIC_REPRESENTATION_ITEM()
RATIONAL_B_SPLINE_CURVE((0.962596973334531,0.966941111578743,1.,0.923879532511287,
1.,0.923879532511287,1.))
REPRESENTATION_ITEM('')
);
#121=(
BOUNDED_CURVE()
B_SPLINE_CURVE(2,(#9590,#9591,#9592,#9593,#9594,#9595,#9596,#9597,#9598),
 .UNSPECIFIED.,.F.,.F.)
B_SPLINE_CURVE_WITH_KNOTS((3,2,2,2,3),(0.0141425757382014,0.025,0.05,0.075,
0.1),.UNSPECIFIED.)
CURVE()
GEOMETRIC_REPRESENTATION_ITEM()
RATIONAL_B_SPLINE_CURVE((0.962596973334531,0.966941111578744,1.,0.923879532511287,
1.,0.923879532511287,1.,0.923879532511287,1.))
REPRESENTATION_ITEM('')
);
#122=(
BOUNDED_CURVE()
B_SPLINE_CURVE(2,(#9894,#9895,#9896),.UNSPECIFIED.,.F.,.F.)
B_SPLINE_CURVE_WITH_KNOTS((3,3),(-1.66699778258505,-0.74828608399493),
 .UNSPECIFIED.)
CURVE()
GEOMETRIC_REPRESENTATION_ITEM()
RATIONAL_B_SPLINE_CURVE((1.84251288693848,2.12755062252262,1.84251288693848))
REPRESENTATION_ITEM('')
);
#123=(
BOUNDED_CURVE()
B_SPLINE_CURVE(2,(#9898,#9899,#9900),.UNSPECIFIED.,.F.,.F.)
B_SPLINE_CURVE_WITH_KNOTS((3,3),(-1.66699778258506,-0.748286083994931),
 .UNSPECIFIED.)
CURVE()
GEOMETRIC_REPRESENTATION_ITEM()
RATIONAL_B_SPLINE_CURVE((1.84251288693848,2.12755062252262,1.84251288693848))
REPRESENTATION_ITEM('')
);
#124=(
BOUNDED_CURVE()
B_SPLINE_CURVE(2,(#9902,#9903,#9904),.UNSPECIFIED.,.F.,.F.)
B_SPLINE_CURVE_WITH_KNOTS((3,3),(-1.66699778258505,-0.748286083994929),
 .UNSPECIFIED.)
CURVE()
GEOMETRIC_REPRESENTATION_ITEM()
RATIONAL_B_SPLINE_CURVE((1.84251288693848,2.12755062252262,1.84251288693848))
REPRESENTATION_ITEM('')
);
#125=(
BOUNDED_CURVE()
B_SPLINE_CURVE(2,(#9906,#9907,#9908),.UNSPECIFIED.,.F.,.F.)
B_SPLINE_CURVE_WITH_KNOTS((3,3),(0.74828608399493,1.20764193328999),
 .UNSPECIFIED.)
CURVE()
GEOMETRIC_REPRESENTATION_ITEM()
RATIONAL_B_SPLINE_CURVE((1.84251288693848,1.98503175473055,1.98503175473055))
REPRESENTATION_ITEM('')
);
#126=(
BOUNDED_CURVE()
B_SPLINE_CURVE(2,(#9913,#9914,#9915),.UNSPECIFIED.,.F.,.F.)
B_SPLINE_CURVE_WITH_KNOTS((3,3),(1.20764193328999,1.66699778258505),
 .UNSPECIFIED.)
CURVE()
GEOMETRIC_REPRESENTATION_ITEM()
RATIONAL_B_SPLINE_CURVE((1.98503175473055,1.98503175473055,1.84251288693848))
REPRESENTATION_ITEM('')
);
#127=(
BOUNDED_CURVE()
B_SPLINE_CURVE(2,(#9917,#9918,#9919),.UNSPECIFIED.,.F.,.F.)
B_SPLINE_CURVE_WITH_KNOTS((3,3),(-1.66699778258506,-0.748286083994931),
 .UNSPECIFIED.)
CURVE()
GEOMETRIC_REPRESENTATION_ITEM()
RATIONAL_B_SPLINE_CURVE((1.84251288693848,2.12755062252262,1.84251288693848))
REPRESENTATION_ITEM('')
);
#128=(
BOUNDED_CURVE()
B_SPLINE_CURVE(2,(#9920,#9921,#9922),.UNSPECIFIED.,.F.,.F.)
B_SPLINE_CURVE_WITH_KNOTS((3,3),(-1.66699778258505,-0.748286083994929),
 .UNSPECIFIED.)
CURVE()
GEOMETRIC_REPRESENTATION_ITEM()
RATIONAL_B_SPLINE_CURVE((1.84251288693848,2.12755062252262,1.84251288693848))
REPRESENTATION_ITEM('')
);
#129=(
BOUNDED_CURVE()
B_SPLINE_CURVE(2,(#10020,#10021,#10022,#10023,#10024,#10025,#10026,#10027,
#10028,#10029,#10030,#10031,#10032,#10033,#10034,#10035,#10036),
 .UNSPECIFIED.,.F.,.F.)
B_SPLINE_CURVE_WITH_KNOTS((3,2,2,2,2,2,2,2,3),(0.1,0.125,0.15,0.175,0.2,
0.225,0.25,0.275,0.3),.UNSPECIFIED.)
CURVE()
GEOMETRIC_REPRESENTATION_ITEM()
RATIONAL_B_SPLINE_CURVE((1.,0.923879532511287,1.,0.923879532511287,1.,0.923879532511287,
1.,0.923879532511287,1.,0.923879532511287,1.,0.923879532511287,1.,0.923879532511287,
1.,0.923879532511287,1.))
REPRESENTATION_ITEM('')
);
#130=(
BOUNDED_CURVE()
B_SPLINE_CURVE(2,(#10037,#10038,#10039,#10040,#10041,#10042,#10043,#10044,
#10045,#10046,#10047,#10048,#10049,#10050,#10051,#10052,#10053),
 .UNSPECIFIED.,.F.,.F.)
B_SPLINE_CURVE_WITH_KNOTS((3,2,2,2,2,2,2,2,3),(0.1,0.125,0.15,0.175,0.2,
0.225,0.25,0.275,0.3),.UNSPECIFIED.)
CURVE()
GEOMETRIC_REPRESENTATION_ITEM()
RATIONAL_B_SPLINE_CURVE((1.,0.923879532511287,1.,0.923879532511287,1.,0.923879532511287,
1.,0.923879532511287,1.,0.923879532511287,1.,0.923879532511287,1.,0.923879532511287,
1.,0.923879532511287,1.))
REPRESENTATION_ITEM('')
);
#131=CONICAL_SURFACE('',#6019,6.5,1.0471975511966);
#132=CONICAL_SURFACE('',#6021,6.5,1.0471975511966);
#133=CONICAL_SURFACE('',#6029,6.5,1.0471975511966);
#134=CONICAL_SURFACE('',#6031,6.5,1.0471975511966);
#135=CONICAL_SURFACE('',#6033,6.5,1.0471975511966);
#136=CONICAL_SURFACE('',#6035,6.5,1.0471975511966);
#137=CONICAL_SURFACE('',#6037,6.5,1.0471975511966);
#138=CONICAL_SURFACE('',#6040,6.5,1.0471975511966);
#139=CONICAL_SURFACE('',#6042,6.5,1.0471975511966);
#140=CONICAL_SURFACE('',#6044,6.5,1.0471975511966);
#141=CONICAL_SURFACE('',#6046,6.5,1.0471975511966);
#142=CONICAL_SURFACE('',#6048,6.5,1.0471975511966);
#143=CONICAL_SURFACE('',#6105,2.008532,0.785398163397448);
#144=CONICAL_SURFACE('',#6108,2.5,0.785398163397448);
#145=CONICAL_SURFACE('',#6115,5.06,1.0471975511966);
#146=CONICAL_SURFACE('',#6117,2.5,0.785398163397448);
#147=CONICAL_SURFACE('',#6119,2.008532,0.785398163397448);
#148=SHAPE_REPRESENTATION_RELATIONSHIP('SRR','None',#10453,#156);
#149=SHAPE_REPRESENTATION_RELATIONSHIP('SRR','None',#10454,#157);
#150=SHAPE_REPRESENTATION_RELATIONSHIP('SRR','None',#10455,#158);
#151=SHAPE_REPRESENTATION_RELATIONSHIP('SRR','None',#10456,#159);
#152=SHAPE_REPRESENTATION_RELATIONSHIP('SRR','None',#10457,#160);
#153=SHAPE_REPRESENTATION_RELATIONSHIP('SRR','None',#10458,#161);
#154=SHAPE_REPRESENTATION_RELATIONSHIP('SRR','None',#10459,#162);
#155=SHAPE_REPRESENTATION_RELATIONSHIP('SRR','None',#10460,#163);
#156=ADVANCED_BREP_SHAPE_REPRESENTATION('',(#172),#10405);
#157=ADVANCED_BREP_SHAPE_REPRESENTATION('',(#173),#10406);
#158=ADVANCED_BREP_SHAPE_REPRESENTATION('',(#174),#10407);
#159=ADVANCED_BREP_SHAPE_REPRESENTATION('',(#175),#10408);
#160=ADVANCED_BREP_SHAPE_REPRESENTATION('',(#176),#10409);
#161=ADVANCED_BREP_SHAPE_REPRESENTATION('',(#177),#10410);
#162=ADVANCED_BREP_SHAPE_REPRESENTATION('',(#178),#10411);
#163=ADVANCED_BREP_SHAPE_REPRESENTATION('',(#179),#10412);
#164=STYLED_ITEM('',(#10502),#172);
#165=STYLED_ITEM('',(#10502),#173);
#166=STYLED_ITEM('',(#10502),#174);
#167=STYLED_ITEM('',(#10503),#175);
#168=STYLED_ITEM('',(#10504),#176);
#169=STYLED_ITEM('',(#10503),#177);
#170=STYLED_ITEM('',(#10502),#178);
#171=STYLED_ITEM('',(#10503),#179);
#172=MANIFOLD_SOLID_BREP('Body1',#5299);
#173=MANIFOLD_SOLID_BREP('Body1',#5300);
#174=MANIFOLD_SOLID_BREP('Body1',#5301);
#175=MANIFOLD_SOLID_BREP('Body1',#5302);
#176=MANIFOLD_SOLID_BREP('Body1',#5303);
#177=MANIFOLD_SOLID_BREP('Body1',#5304);
#178=MANIFOLD_SOLID_BREP('Body1',#5305);
#179=MANIFOLD_SOLID_BREP('Body1',#5306);
#180=FACE_BOUND('',#575,.T.);
#181=FACE_BOUND('',#576,.T.);
#182=FACE_BOUND('',#577,.T.);
#183=FACE_BOUND('',#578,.T.);
#184=FACE_BOUND('',#579,.T.);
#185=FACE_BOUND('',#581,.T.);
#186=FACE_BOUND('',#582,.T.);
#187=FACE_BOUND('',#583,.T.);
#188=FACE_BOUND('',#584,.T.);
#189=FACE_BOUND('',#585,.T.);
#190=FACE_BOUND('',#589,.T.);
#191=FACE_BOUND('',#591,.T.);
#192=FACE_BOUND('',#594,.T.);
#193=FACE_BOUND('',#595,.T.);
#194=FACE_BOUND('',#597,.T.);
#195=FACE_BOUND('',#598,.T.);
#196=FACE_BOUND('',#606,.T.);
#197=FACE_BOUND('',#608,.T.);
#198=FACE_BOUND('',#611,.T.);
#199=FACE_BOUND('',#668,.T.);
#200=FACE_BOUND('',#670,.T.);
#201=FACE_BOUND('',#822,.T.);
#202=FACE_BOUND('',#829,.T.);
#203=FACE_BOUND('',#838,.T.);
#204=FACE_BOUND('',#839,.T.);
#205=FACE_BOUND('',#840,.T.);
#206=FACE_BOUND('',#841,.T.);
#207=FACE_BOUND('',#842,.T.);
#208=FACE_BOUND('',#844,.T.);
#209=FACE_BOUND('',#845,.T.);
#210=FACE_BOUND('',#846,.T.);
#211=FACE_BOUND('',#847,.T.);
#212=FACE_BOUND('',#848,.T.);
#213=FACE_BOUND('',#850,.T.);
#214=FACE_BOUND('',#854,.T.);
#215=FACE_BOUND('',#856,.T.);
#216=FACE_BOUND('',#859,.T.);
#217=FACE_BOUND('',#882,.T.);
#218=FACE_BOUND('',#884,.T.);
#219=PLANE('',#5425);
#220=PLANE('',#5426);
#221=PLANE('',#5427);
#222=PLANE('',#5428);
#223=PLANE('',#5429);
#224=PLANE('',#5430);
#225=PLANE('',#5431);
#226=PLANE('',#5432);
#227=PLANE('',#5433);
#228=PLANE('',#5434);
#229=PLANE('',#5455);
#230=PLANE('',#5456);
#231=PLANE('',#5457);
#232=PLANE('',#5458);
#233=PLANE('',#5459);
#234=PLANE('',#5460);
#235=PLANE('',#5461);
#236=PLANE('',#5462);
#237=PLANE('',#5463);
#238=PLANE('',#5464);
#239=PLANE('',#5465);
#240=PLANE('',#5611);
#241=PLANE('',#5745);
#242=PLANE('',#6012);
#243=PLANE('',#6013);
#244=PLANE('',#6014);
#245=PLANE('',#6023);
#246=PLANE('',#6024);
#247=PLANE('',#6025);
#248=PLANE('',#6026);
#249=PLANE('',#6027);
#250=PLANE('',#6028);
#251=PLANE('',#6039);
#252=PLANE('',#6050);
#253=PLANE('',#6073);
#254=PLANE('',#6074);
#255=PLANE('',#6075);
#256=PLANE('',#6083);
#257=PLANE('',#6084);
#258=PLANE('',#6089);
#259=PLANE('',#6090);
#260=PLANE('',#6091);
#261=PLANE('',#6092);
#262=PLANE('',#6093);
#263=PLANE('',#6094);
#264=PLANE('',#6095);
#265=PLANE('',#6096);
#266=PLANE('',#6097);
#267=PLANE('',#6121);
#268=PLANE('',#6124);
#269=PLANE('',#6127);
#270=PLANE('',#6128);
#271=PLANE('',#6129);
#272=PLANE('',#6130);
#273=PLANE('',#6131);
#274=PLANE('',#6132);
#275=FACE_OUTER_BOUND('',#565,.T.);
#276=FACE_OUTER_BOUND('',#566,.T.);
#277=FACE_OUTER_BOUND('',#567,.T.);
#278=FACE_OUTER_BOUND('',#568,.T.);
#279=FACE_OUTER_BOUND('',#569,.T.);
#280=FACE_OUTER_BOUND('',#570,.T.);
#281=FACE_OUTER_BOUND('',#571,.T.);
#282=FACE_OUTER_BOUND('',#572,.T.);
#283=FACE_OUTER_BOUND('',#573,.T.);
#284=FACE_OUTER_BOUND('',#574,.T.);
#285=FACE_OUTER_BOUND('',#580,.T.);
#286=FACE_OUTER_BOUND('',#586,.T.);
#287=FACE_OUTER_BOUND('',#587,.T.);
#288=FACE_OUTER_BOUND('',#588,.T.);
#289=FACE_OUTER_BOUND('',#590,.T.);
#290=FACE_OUTER_BOUND('',#592,.T.);
#291=FACE_OUTER_BOUND('',#593,.T.);
#292=FACE_OUTER_BOUND('',#596,.T.);
#293=FACE_OUTER_BOUND('',#599,.T.);
#294=FACE_OUTER_BOUND('',#600,.T.);
#295=FACE_OUTER_BOUND('',#601,.T.);
#296=FACE_OUTER_BOUND('',#602,.T.);
#297=FACE_OUTER_BOUND('',#603,.T.);
#298=FACE_OUTER_BOUND('',#604,.T.);
#299=FACE_OUTER_BOUND('',#605,.T.);
#300=FACE_OUTER_BOUND('',#607,.T.);
#301=FACE_OUTER_BOUND('',#609,.T.);
#302=FACE_OUTER_BOUND('',#610,.T.);
#303=FACE_OUTER_BOUND('',#612,.T.);
#304=FACE_OUTER_BOUND('',#613,.T.);
#305=FACE_OUTER_BOUND('',#614,.T.);
#306=FACE_OUTER_BOUND('',#615,.T.);
#307=FACE_OUTER_BOUND('',#616,.T.);
#308=FACE_OUTER_BOUND('',#617,.T.);
#309=FACE_OUTER_BOUND('',#618,.T.);
#310=FACE_OUTER_BOUND('',#619,.T.);
#311=FACE_OUTER_BOUND('',#620,.T.);
#312=FACE_OUTER_BOUND('',#621,.T.);
#313=FACE_OUTER_BOUND('',#622,.T.);
#314=FACE_OUTER_BOUND('',#623,.T.);
#315=FACE_OUTER_BOUND('',#624,.T.);
#316=FACE_OUTER_BOUND('',#625,.T.);
#317=FACE_OUTER_BOUND('',#626,.T.);
#318=FACE_OUTER_BOUND('',#627,.T.);
#319=FACE_OUTER_BOUND('',#628,.T.);
#320=FACE_OUTER_BOUND('',#629,.T.);
#321=FACE_OUTER_BOUND('',#630,.T.);
#322=FACE_OUTER_BOUND('',#631,.T.);
#323=FACE_OUTER_BOUND('',#632,.T.);
#324=FACE_OUTER_BOUND('',#633,.T.);
#325=FACE_OUTER_BOUND('',#634,.T.);
#326=FACE_OUTER_BOUND('',#635,.T.);
#327=FACE_OUTER_BOUND('',#636,.T.);
#328=FACE_OUTER_BOUND('',#637,.T.);
#329=FACE_OUTER_BOUND('',#638,.T.);
#330=FACE_OUTER_BOUND('',#639,.T.);
#331=FACE_OUTER_BOUND('',#640,.T.);
#332=FACE_OUTER_BOUND('',#641,.T.);
#333=FACE_OUTER_BOUND('',#642,.T.);
#334=FACE_OUTER_BOUND('',#643,.T.);
#335=FACE_OUTER_BOUND('',#644,.T.);
#336=FACE_OUTER_BOUND('',#645,.T.);
#337=FACE_OUTER_BOUND('',#646,.T.);
#338=FACE_OUTER_BOUND('',#647,.T.);
#339=FACE_OUTER_BOUND('',#648,.T.);
#340=FACE_OUTER_BOUND('',#649,.T.);
#341=FACE_OUTER_BOUND('',#650,.T.);
#342=FACE_OUTER_BOUND('',#651,.T.);
#343=FACE_OUTER_BOUND('',#652,.T.);
#344=FACE_OUTER_BOUND('',#653,.T.);
#345=FACE_OUTER_BOUND('',#654,.T.);
#346=FACE_OUTER_BOUND('',#655,.T.);
#347=FACE_OUTER_BOUND('',#656,.T.);
#348=FACE_OUTER_BOUND('',#657,.T.);
#349=FACE_OUTER_BOUND('',#658,.T.);
#350=FACE_OUTER_BOUND('',#659,.T.);
#351=FACE_OUTER_BOUND('',#660,.T.);
#352=FACE_OUTER_BOUND('',#661,.T.);
#353=FACE_OUTER_BOUND('',#662,.T.);
#354=FACE_OUTER_BOUND('',#663,.T.);
#355=FACE_OUTER_BOUND('',#664,.T.);
#356=FACE_OUTER_BOUND('',#665,.T.);
#357=FACE_OUTER_BOUND('',#666,.T.);
#358=FACE_OUTER_BOUND('',#667,.T.);
#359=FACE_OUTER_BOUND('',#669,.T.);
#360=FACE_OUTER_BOUND('',#671,.T.);
#361=FACE_OUTER_BOUND('',#672,.T.);
#362=FACE_OUTER_BOUND('',#673,.T.);
#363=FACE_OUTER_BOUND('',#674,.T.);
#364=FACE_OUTER_BOUND('',#675,.T.);
#365=FACE_OUTER_BOUND('',#676,.T.);
#366=FACE_OUTER_BOUND('',#677,.T.);
#367=FACE_OUTER_BOUND('',#678,.T.);
#368=FACE_OUTER_BOUND('',#679,.T.);
#369=FACE_OUTER_BOUND('',#680,.T.);
#370=FACE_OUTER_BOUND('',#681,.T.);
#371=FACE_OUTER_BOUND('',#682,.T.);
#372=FACE_OUTER_BOUND('',#683,.T.);
#373=FACE_OUTER_BOUND('',#684,.T.);
#374=FACE_OUTER_BOUND('',#685,.T.);
#375=FACE_OUTER_BOUND('',#686,.T.);
#376=FACE_OUTER_BOUND('',#687,.T.);
#377=FACE_OUTER_BOUND('',#688,.T.);
#378=FACE_OUTER_BOUND('',#689,.T.);
#379=FACE_OUTER_BOUND('',#690,.T.);
#380=FACE_OUTER_BOUND('',#691,.T.);
#381=FACE_OUTER_BOUND('',#692,.T.);
#382=FACE_OUTER_BOUND('',#693,.T.);
#383=FACE_OUTER_BOUND('',#694,.T.);
#384=FACE_OUTER_BOUND('',#695,.T.);
#385=FACE_OUTER_BOUND('',#696,.T.);
#386=FACE_OUTER_BOUND('',#697,.T.);
#387=FACE_OUTER_BOUND('',#698,.T.);
#388=FACE_OUTER_BOUND('',#699,.T.);
#389=FACE_OUTER_BOUND('',#700,.T.);
#390=FACE_OUTER_BOUND('',#701,.T.);
#391=FACE_OUTER_BOUND('',#702,.T.);
#392=FACE_OUTER_BOUND('',#703,.T.);
#393=FACE_OUTER_BOUND('',#704,.T.);
#394=FACE_OUTER_BOUND('',#705,.T.);
#395=FACE_OUTER_BOUND('',#706,.T.);
#396=FACE_OUTER_BOUND('',#707,.T.);
#397=FACE_OUTER_BOUND('',#708,.T.);
#398=FACE_OUTER_BOUND('',#709,.T.);
#399=FACE_OUTER_BOUND('',#710,.T.);
#400=FACE_OUTER_BOUND('',#711,.T.);
#401=FACE_OUTER_BOUND('',#712,.T.);
#402=FACE_OUTER_BOUND('',#713,.T.);
#403=FACE_OUTER_BOUND('',#714,.T.);
#404=FACE_OUTER_BOUND('',#715,.T.);
#405=FACE_OUTER_BOUND('',#716,.T.);
#406=FACE_OUTER_BOUND('',#717,.T.);
#407=FACE_OUTER_BOUND('',#718,.T.);
#408=FACE_OUTER_BOUND('',#719,.T.);
#409=FACE_OUTER_BOUND('',#720,.T.);
#410=FACE_OUTER_BOUND('',#721,.T.);
#411=FACE_OUTER_BOUND('',#722,.T.);
#412=FACE_OUTER_BOUND('',#723,.T.);
#413=FACE_OUTER_BOUND('',#724,.T.);
#414=FACE_OUTER_BOUND('',#725,.T.);
#415=FACE_OUTER_BOUND('',#726,.T.);
#416=FACE_OUTER_BOUND('',#727,.T.);
#417=FACE_OUTER_BOUND('',#728,.T.);
#418=FACE_OUTER_BOUND('',#729,.T.);
#419=FACE_OUTER_BOUND('',#730,.T.);
#420=FACE_OUTER_BOUND('',#731,.T.);
#421=FACE_OUTER_BOUND('',#732,.T.);
#422=FACE_OUTER_BOUND('',#733,.T.);
#423=FACE_OUTER_BOUND('',#734,.T.);
#424=FACE_OUTER_BOUND('',#735,.T.);
#425=FACE_OUTER_BOUND('',#736,.T.);
#426=FACE_OUTER_BOUND('',#737,.T.);
#427=FACE_OUTER_BOUND('',#738,.T.);
#428=FACE_OUTER_BOUND('',#739,.T.);
#429=FACE_OUTER_BOUND('',#740,.T.);
#430=FACE_OUTER_BOUND('',#741,.T.);
#431=FACE_OUTER_BOUND('',#742,.T.);
#432=FACE_OUTER_BOUND('',#743,.T.);
#433=FACE_OUTER_BOUND('',#744,.T.);
#434=FACE_OUTER_BOUND('',#745,.T.);
#435=FACE_OUTER_BOUND('',#746,.T.);
#436=FACE_OUTER_BOUND('',#747,.T.);
#437=FACE_OUTER_BOUND('',#748,.T.);
#438=FACE_OUTER_BOUND('',#749,.T.);
#439=FACE_OUTER_BOUND('',#750,.T.);
#440=FACE_OUTER_BOUND('',#751,.T.);
#441=FACE_OUTER_BOUND('',#752,.T.);
#442=FACE_OUTER_BOUND('',#753,.T.);
#443=FACE_OUTER_BOUND('',#754,.T.);
#444=FACE_OUTER_BOUND('',#755,.T.);
#445=FACE_OUTER_BOUND('',#756,.T.);
#446=FACE_OUTER_BOUND('',#757,.T.);
#447=FACE_OUTER_BOUND('',#758,.T.);
#448=FACE_OUTER_BOUND('',#759,.T.);
#449=FACE_OUTER_BOUND('',#760,.T.);
#450=FACE_OUTER_BOUND('',#761,.T.);
#451=FACE_OUTER_BOUND('',#762,.T.);
#452=FACE_OUTER_BOUND('',#763,.T.);
#453=FACE_OUTER_BOUND('',#764,.T.);
#454=FACE_OUTER_BOUND('',#765,.T.);
#455=FACE_OUTER_BOUND('',#766,.T.);
#456=FACE_OUTER_BOUND('',#767,.T.);
#457=FACE_OUTER_BOUND('',#768,.T.);
#458=FACE_OUTER_BOUND('',#769,.T.);
#459=FACE_OUTER_BOUND('',#770,.T.);
#460=FACE_OUTER_BOUND('',#771,.T.);
#461=FACE_OUTER_BOUND('',#772,.T.);
#462=FACE_OUTER_BOUND('',#773,.T.);
#463=FACE_OUTER_BOUND('',#774,.T.);
#464=FACE_OUTER_BOUND('',#775,.T.);
#465=FACE_OUTER_BOUND('',#776,.T.);
#466=FACE_OUTER_BOUND('',#777,.T.);
#467=FACE_OUTER_BOUND('',#778,.T.);
#468=FACE_OUTER_BOUND('',#779,.T.);
#469=FACE_OUTER_BOUND('',#780,.T.);
#470=FACE_OUTER_BOUND('',#781,.T.);
#471=FACE_OUTER_BOUND('',#782,.T.);
#472=FACE_OUTER_BOUND('',#783,.T.);
#473=FACE_OUTER_BOUND('',#784,.T.);
#474=FACE_OUTER_BOUND('',#785,.T.);
#475=FACE_OUTER_BOUND('',#786,.T.);
#476=FACE_OUTER_BOUND('',#787,.T.);
#477=FACE_OUTER_BOUND('',#788,.T.);
#478=FACE_OUTER_BOUND('',#789,.T.);
#479=FACE_OUTER_BOUND('',#790,.T.);
#480=FACE_OUTER_BOUND('',#791,.T.);
#481=FACE_OUTER_BOUND('',#792,.T.);
#482=FACE_OUTER_BOUND('',#793,.T.);
#483=FACE_OUTER_BOUND('',#794,.T.);
#484=FACE_OUTER_BOUND('',#795,.T.);
#485=FACE_OUTER_BOUND('',#796,.T.);
#486=FACE_OUTER_BOUND('',#797,.T.);
#487=FACE_OUTER_BOUND('',#798,.T.);
#488=FACE_OUTER_BOUND('',#799,.T.);
#489=FACE_OUTER_BOUND('',#800,.T.);
#490=FACE_OUTER_BOUND('',#801,.T.);
#491=FACE_OUTER_BOUND('',#802,.T.);
#492=FACE_OUTER_BOUND('',#803,.T.);
#493=FACE_OUTER_BOUND('',#804,.T.);
#494=FACE_OUTER_BOUND('',#805,.T.);
#495=FACE_OUTER_BOUND('',#806,.T.);
#496=FACE_OUTER_BOUND('',#807,.T.);
#497=FACE_OUTER_BOUND('',#808,.T.);
#498=FACE_OUTER_BOUND('',#809,.T.);
#499=FACE_OUTER_BOUND('',#810,.T.);
#500=FACE_OUTER_BOUND('',#811,.T.);
#501=FACE_OUTER_BOUND('',#812,.T.);
#502=FACE_OUTER_BOUND('',#813,.T.);
#503=FACE_OUTER_BOUND('',#814,.T.);
#504=FACE_OUTER_BOUND('',#815,.T.);
#505=FACE_OUTER_BOUND('',#816,.T.);
#506=FACE_OUTER_BOUND('',#817,.T.);
#507=FACE_OUTER_BOUND('',#818,.T.);
#508=FACE_OUTER_BOUND('',#819,.T.);
#509=FACE_OUTER_BOUND('',#820,.T.);
#510=FACE_OUTER_BOUND('',#821,.T.);
#511=FACE_OUTER_BOUND('',#823,.T.);
#512=FACE_OUTER_BOUND('',#824,.T.);
#513=FACE_OUTER_BOUND('',#825,.T.);
#514=FACE_OUTER_BOUND('',#826,.T.);
#515=FACE_OUTER_BOUND('',#827,.T.);
#516=FACE_OUTER_BOUND('',#828,.T.);
#517=FACE_OUTER_BOUND('',#830,.T.);
#518=FACE_OUTER_BOUND('',#831,.T.);
#519=FACE_OUTER_BOUND('',#832,.T.);
#520=FACE_OUTER_BOUND('',#833,.T.);
#521=FACE_OUTER_BOUND('',#834,.T.);
#522=FACE_OUTER_BOUND('',#835,.T.);
#523=FACE_OUTER_BOUND('',#836,.T.);
#524=FACE_OUTER_BOUND('',#837,.T.);
#525=FACE_OUTER_BOUND('',#843,.T.);
#526=FACE_OUTER_BOUND('',#849,.T.);
#527=FACE_OUTER_BOUND('',#851,.T.);
#528=FACE_OUTER_BOUND('',#852,.T.);
#529=FACE_OUTER_BOUND('',#853,.T.);
#530=FACE_OUTER_BOUND('',#855,.T.);
#531=FACE_OUTER_BOUND('',#857,.T.);
#532=FACE_OUTER_BOUND('',#858,.T.);
#533=FACE_OUTER_BOUND('',#860,.T.);
#534=FACE_OUTER_BOUND('',#861,.T.);
#535=FACE_OUTER_BOUND('',#862,.T.);
#536=FACE_OUTER_BOUND('',#863,.T.);
#537=FACE_OUTER_BOUND('',#864,.T.);
#538=FACE_OUTER_BOUND('',#865,.T.);
#539=FACE_OUTER_BOUND('',#866,.T.);
#540=FACE_OUTER_BOUND('',#867,.T.);
#541=FACE_OUTER_BOUND('',#868,.T.);
#542=FACE_OUTER_BOUND('',#869,.T.);
#543=FACE_OUTER_BOUND('',#870,.T.);
#544=FACE_OUTER_BOUND('',#871,.T.);
#545=FACE_OUTER_BOUND('',#872,.T.);
#546=FACE_OUTER_BOUND('',#873,.T.);
#547=FACE_OUTER_BOUND('',#874,.T.);
#548=FACE_OUTER_BOUND('',#875,.T.);
#549=FACE_OUTER_BOUND('',#876,.T.);
#550=FACE_OUTER_BOUND('',#877,.T.);
#551=FACE_OUTER_BOUND('',#878,.T.);
#552=FACE_OUTER_BOUND('',#879,.T.);
#553=FACE_OUTER_BOUND('',#880,.T.);
#554=FACE_OUTER_BOUND('',#881,.T.);
#555=FACE_OUTER_BOUND('',#883,.T.);
#556=FACE_OUTER_BOUND('',#885,.T.);
#557=FACE_OUTER_BOUND('',#886,.T.);
#558=FACE_OUTER_BOUND('',#887,.T.);
#559=FACE_OUTER_BOUND('',#888,.T.);
#560=FACE_OUTER_BOUND('',#889,.T.);
#561=FACE_OUTER_BOUND('',#890,.T.);
#562=FACE_OUTER_BOUND('',#891,.T.);
#563=FACE_OUTER_BOUND('',#892,.T.);
#564=FACE_OUTER_BOUND('',#893,.T.);
#565=EDGE_LOOP('',(#3222,#3223,#3224,#3225));
#566=EDGE_LOOP('',(#3226,#3227,#3228,#3229));
#567=EDGE_LOOP('',(#3230,#3231,#3232,#3233));
#568=EDGE_LOOP('',(#3234,#3235,#3236,#3237));
#569=EDGE_LOOP('',(#3238,#3239,#3240,#3241));
#570=EDGE_LOOP('',(#3242,#3243,#3244,#3245));
#571=EDGE_LOOP('',(#3246,#3247,#3248,#3249));
#572=EDGE_LOOP('',(#3250,#3251,#3252,#3253));
#573=EDGE_LOOP('',(#3254,#3255,#3256,#3257));
#574=EDGE_LOOP('',(#3258,#3259,#3260,#3261));
#575=EDGE_LOOP('',(#3262));
#576=EDGE_LOOP('',(#3263));
#577=EDGE_LOOP('',(#3264));
#578=EDGE_LOOP('',(#3265));
#579=EDGE_LOOP('',(#3266));
#580=EDGE_LOOP('',(#3267,#3268,#3269,#3270));
#581=EDGE_LOOP('',(#3271));
#582=EDGE_LOOP('',(#3272));
#583=EDGE_LOOP('',(#3273));
#584=EDGE_LOOP('',(#3274));
#585=EDGE_LOOP('',(#3275));
#586=EDGE_LOOP('',(#3276,#3277,#3278,#3279,#3280,#3281));
#587=EDGE_LOOP('',(#3282,#3283,#3284,#3285,#3286,#3287));
#588=EDGE_LOOP('',(#3288));
#589=EDGE_LOOP('',(#3289));
#590=EDGE_LOOP('',(#3290));
#591=EDGE_LOOP('',(#3291));
#592=EDGE_LOOP('',(#3292,#3293,#3294,#3295));
#593=EDGE_LOOP('',(#3296,#3297,#3298,#3299));
#594=EDGE_LOOP('',(#3300));
#595=EDGE_LOOP('',(#3301));
#596=EDGE_LOOP('',(#3302,#3303,#3304,#3305));
#597=EDGE_LOOP('',(#3306));
#598=EDGE_LOOP('',(#3307));
#599=EDGE_LOOP('',(#3308,#3309,#3310,#3311));
#600=EDGE_LOOP('',(#3312,#3313,#3314,#3315));
#601=EDGE_LOOP('',(#3316,#3317,#3318,#3319,#3320,#3321,#3322,#3323));
#602=EDGE_LOOP('',(#3324,#3325,#3326,#3327,#3328,#3329));
#603=EDGE_LOOP('',(#3330,#3331,#3332,#3333));
#604=EDGE_LOOP('',(#3334,#3335,#3336,#3337));
#605=EDGE_LOOP('',(#3338));
#606=EDGE_LOOP('',(#3339));
#607=EDGE_LOOP('',(#3340));
#608=EDGE_LOOP('',(#3341));
#609=EDGE_LOOP('',(#3342));
#610=EDGE_LOOP('',(#3343));
#611=EDGE_LOOP('',(#3344));
#612=EDGE_LOOP('',(#3345,#3346,#3347,#3348,#3349,#3350));
#613=EDGE_LOOP('',(#3351,#3352,#3353,#3354));
#614=EDGE_LOOP('',(#3355,#3356,#3357,#3358,#3359));
#615=EDGE_LOOP('',(#3360,#3361,#3362,#3363));
#616=EDGE_LOOP('',(#3364,#3365,#3366,#3367,#3368));
#617=EDGE_LOOP('',(#3369,#3370,#3371,#3372));
#618=EDGE_LOOP('',(#3373));
#619=EDGE_LOOP('',(#3374,#3375,#3376,#3377));
#620=EDGE_LOOP('',(#3378,#3379,#3380,#3381));
#621=EDGE_LOOP('',(#3382,#3383,#3384,#3385));
#622=EDGE_LOOP('',(#3386,#3387,#3388,#3389));
#623=EDGE_LOOP('',(#3390,#3391,#3392,#3393));
#624=EDGE_LOOP('',(#3394,#3395,#3396,#3397));
#625=EDGE_LOOP('',(#3398,#3399,#3400,#3401));
#626=EDGE_LOOP('',(#3402,#3403,#3404,#3405));
#627=EDGE_LOOP('',(#3406,#3407,#3408,#3409));
#628=EDGE_LOOP('',(#3410,#3411,#3412,#3413));
#629=EDGE_LOOP('',(#3414,#3415,#3416,#3417));
#630=EDGE_LOOP('',(#3418,#3419,#3420,#3421));
#631=EDGE_LOOP('',(#3422,#3423,#3424,#3425));
#632=EDGE_LOOP('',(#3426,#3427,#3428,#3429));
#633=EDGE_LOOP('',(#3430,#3431,#3432,#3433));
#634=EDGE_LOOP('',(#3434,#3435,#3436,#3437));
#635=EDGE_LOOP('',(#3438,#3439,#3440,#3441));
#636=EDGE_LOOP('',(#3442,#3443,#3444,#3445));
#637=EDGE_LOOP('',(#3446,#3447,#3448,#3449));
#638=EDGE_LOOP('',(#3450,#3451,#3452,#3453));
#639=EDGE_LOOP('',(#3454,#3455,#3456,#3457));
#640=EDGE_LOOP('',(#3458,#3459,#3460,#3461));
#641=EDGE_LOOP('',(#3462,#3463,#3464,#3465));
#642=EDGE_LOOP('',(#3466,#3467,#3468,#3469));
#643=EDGE_LOOP('',(#3470,#3471,#3472,#3473));
#644=EDGE_LOOP('',(#3474,#3475,#3476,#3477));
#645=EDGE_LOOP('',(#3478,#3479,#3480,#3481));
#646=EDGE_LOOP('',(#3482,#3483,#3484,#3485));
#647=EDGE_LOOP('',(#3486,#3487,#3488,#3489));
#648=EDGE_LOOP('',(#3490,#3491,#3492,#3493));
#649=EDGE_LOOP('',(#3494,#3495,#3496,#3497));
#650=EDGE_LOOP('',(#3498,#3499,#3500,#3501));
#651=EDGE_LOOP('',(#3502,#3503,#3504,#3505));
#652=EDGE_LOOP('',(#3506,#3507,#3508,#3509));
#653=EDGE_LOOP('',(#3510,#3511,#3512,#3513));
#654=EDGE_LOOP('',(#3514,#3515,#3516,#3517));
#655=EDGE_LOOP('',(#3518,#3519,#3520,#3521));
#656=EDGE_LOOP('',(#3522,#3523,#3524,#3525));
#657=EDGE_LOOP('',(#3526,#3527,#3528,#3529));
#658=EDGE_LOOP('',(#3530,#3531,#3532,#3533));
#659=EDGE_LOOP('',(#3534,#3535,#3536,#3537));
#660=EDGE_LOOP('',(#3538,#3539,#3540,#3541));
#661=EDGE_LOOP('',(#3542,#3543,#3544,#3545));
#662=EDGE_LOOP('',(#3546,#3547,#3548,#3549));
#663=EDGE_LOOP('',(#3550,#3551,#3552,#3553));
#664=EDGE_LOOP('',(#3554,#3555,#3556,#3557));
#665=EDGE_LOOP('',(#3558,#3559,#3560,#3561));
#666=EDGE_LOOP('',(#3562,#3563,#3564,#3565));
#667=EDGE_LOOP('',(#3566,#3567,#3568,#3569,#3570,#3571,#3572,#3573,#3574,
#3575,#3576,#3577,#3578,#3579,#3580,#3581,#3582,#3583,#3584,#3585,#3586,
#3587,#3588,#3589,#3590,#3591,#3592,#3593,#3594,#3595,#3596,#3597,#3598,
#3599,#3600,#3601,#3602,#3603,#3604,#3605,#3606,#3607,#3608,#3609,#3610,
#3611,#3612,#3613,#3614,#3615,#3616,#3617,#3618,#3619,#3620,#3621,#3622,
#3623,#3624,#3625,#3626,#3627,#3628,#3629,#3630,#3631,#3632,#3633,#3634,
#3635,#3636,#3637,#3638,#3639,#3640,#3641,#3642,#3643,#3644,#3645,#3646,
#3647,#3648,#3649,#3650,#3651,#3652,#3653,#3654,#3655,#3656,#3657,#3658,
#3659,#3660,#3661,#3662,#3663,#3664,#3665,#3666,#3667,#3668,#3669,#3670,
#3671,#3672,#3673,#3674,#3675,#3676,#3677,#3678,#3679,#3680,#3681,#3682,
#3683,#3684,#3685,#3686,#3687,#3688,#3689,#3690,#3691,#3692,#3693,#3694,
#3695,#3696,#3697,#3698,#3699,#3700,#3701,#3702,#3703,#3704,#3705,#3706,
#3707,#3708,#3709,#3710,#3711,#3712,#3713,#3714,#3715,#3716,#3717,#3718,
#3719,#3720,#3721,#3722,#3723,#3724,#3725,#3726,#3727,#3728,#3729,#3730,
#3731,#3732,#3733,#3734,#3735,#3736,#3737,#3738,#3739,#3740,#3741,#3742,
#3743,#3744,#3745));
#668=EDGE_LOOP('',(#3746,#3747,#3748,#3749));
#669=EDGE_LOOP('',(#3750,#3751,#3752,#3753,#3754,#3755,#3756,#3757,#3758,
#3759,#3760,#3761,#3762,#3763,#3764,#3765,#3766,#3767,#3768,#3769,#3770,
#3771,#3772,#3773,#3774,#3775,#3776,#3777,#3778,#3779,#3780,#3781,#3782,
#3783,#3784,#3785,#3786,#3787,#3788,#3789,#3790,#3791,#3792,#3793,#3794,
#3795,#3796,#3797,#3798,#3799,#3800,#3801,#3802,#3803,#3804,#3805,#3806,
#3807,#3808,#3809,#3810,#3811,#3812,#3813,#3814,#3815,#3816,#3817,#3818,
#3819,#3820,#3821,#3822,#3823,#3824,#3825,#3826,#3827,#3828,#3829,#3830,
#3831,#3832,#3833,#3834,#3835,#3836,#3837,#3838,#3839,#3840,#3841,#3842,
#3843,#3844,#3845,#3846,#3847,#3848,#3849,#3850,#3851,#3852,#3853,#3854,
#3855,#3856,#3857,#3858,#3859,#3860,#3861,#3862,#3863,#3864,#3865,#3866,
#3867,#3868,#3869,#3870,#3871,#3872,#3873,#3874,#3875,#3876,#3877,#3878,
#3879,#3880,#3881,#3882,#3883,#3884,#3885,#3886,#3887,#3888,#3889,#3890,
#3891,#3892,#3893,#3894,#3895,#3896,#3897,#3898,#3899,#3900,#3901,#3902,
#3903,#3904,#3905,#3906,#3907,#3908,#3909,#3910,#3911,#3912,#3913,#3914,
#3915,#3916,#3917,#3918,#3919,#3920,#3921,#3922,#3923,#3924,#3925,#3926,
#3927,#3928,#3929));
#670=EDGE_LOOP('',(#3930,#3931,#3932,#3933));
#671=EDGE_LOOP('',(#3934,#3935,#3936,#3937));
#672=EDGE_LOOP('',(#3938,#3939,#3940,#3941));
#673=EDGE_LOOP('',(#3942,#3943,#3944,#3945));
#674=EDGE_LOOP('',(#3946,#3947,#3948,#3949));
#675=EDGE_LOOP('',(#3950,#3951,#3952,#3953));
#676=EDGE_LOOP('',(#3954,#3955,#3956,#3957));
#677=EDGE_LOOP('',(#3958,#3959,#3960,#3961));
#678=EDGE_LOOP('',(#3962,#3963,#3964,#3965));
#679=EDGE_LOOP('',(#3966,#3967,#3968,#3969));
#680=EDGE_LOOP('',(#3970,#3971,#3972,#3973));
#681=EDGE_LOOP('',(#3974,#3975,#3976,#3977));
#682=EDGE_LOOP('',(#3978,#3979,#3980,#3981));
#683=EDGE_LOOP('',(#3982,#3983,#3984,#3985));
#684=EDGE_LOOP('',(#3986,#3987,#3988,#3989));
#685=EDGE_LOOP('',(#3990,#3991,#3992,#3993));
#686=EDGE_LOOP('',(#3994,#3995,#3996,#3997));
#687=EDGE_LOOP('',(#3998,#3999,#4000,#4001));
#688=EDGE_LOOP('',(#4002,#4003,#4004,#4005));
#689=EDGE_LOOP('',(#4006,#4007,#4008,#4009));
#690=EDGE_LOOP('',(#4010,#4011,#4012,#4013));
#691=EDGE_LOOP('',(#4014,#4015,#4016,#4017));
#692=EDGE_LOOP('',(#4018,#4019,#4020,#4021));
#693=EDGE_LOOP('',(#4022,#4023,#4024,#4025));
#694=EDGE_LOOP('',(#4026,#4027,#4028,#4029));
#695=EDGE_LOOP('',(#4030,#4031,#4032,#4033));
#696=EDGE_LOOP('',(#4034,#4035,#4036,#4037));
#697=EDGE_LOOP('',(#4038,#4039,#4040,#4041));
#698=EDGE_LOOP('',(#4042,#4043,#4044,#4045));
#699=EDGE_LOOP('',(#4046,#4047,#4048,#4049));
#700=EDGE_LOOP('',(#4050,#4051,#4052,#4053));
#701=EDGE_LOOP('',(#4054,#4055,#4056,#4057));
#702=EDGE_LOOP('',(#4058,#4059,#4060,#4061));
#703=EDGE_LOOP('',(#4062,#4063,#4064,#4065));
#704=EDGE_LOOP('',(#4066,#4067,#4068,#4069));
#705=EDGE_LOOP('',(#4070,#4071,#4072,#4073));
#706=EDGE_LOOP('',(#4074,#4075,#4076,#4077));
#707=EDGE_LOOP('',(#4078,#4079,#4080,#4081));
#708=EDGE_LOOP('',(#4082,#4083,#4084,#4085));
#709=EDGE_LOOP('',(#4086,#4087,#4088,#4089));
#710=EDGE_LOOP('',(#4090,#4091,#4092,#4093));
#711=EDGE_LOOP('',(#4094,#4095,#4096,#4097));
#712=EDGE_LOOP('',(#4098,#4099,#4100,#4101));
#713=EDGE_LOOP('',(#4102,#4103,#4104,#4105));
#714=EDGE_LOOP('',(#4106,#4107,#4108,#4109));
#715=EDGE_LOOP('',(#4110,#4111,#4112,#4113));
#716=EDGE_LOOP('',(#4114,#4115,#4116,#4117));
#717=EDGE_LOOP('',(#4118,#4119,#4120,#4121));
#718=EDGE_LOOP('',(#4122,#4123,#4124,#4125));
#719=EDGE_LOOP('',(#4126,#4127,#4128,#4129));
#720=EDGE_LOOP('',(#4130,#4131,#4132,#4133));
#721=EDGE_LOOP('',(#4134,#4135,#4136,#4137));
#722=EDGE_LOOP('',(#4138,#4139,#4140,#4141));
#723=EDGE_LOOP('',(#4142,#4143,#4144,#4145));
#724=EDGE_LOOP('',(#4146,#4147,#4148,#4149));
#725=EDGE_LOOP('',(#4150,#4151,#4152,#4153));
#726=EDGE_LOOP('',(#4154,#4155,#4156,#4157));
#727=EDGE_LOOP('',(#4158,#4159,#4160,#4161));
#728=EDGE_LOOP('',(#4162,#4163,#4164,#4165));
#729=EDGE_LOOP('',(#4166,#4167,#4168,#4169));
#730=EDGE_LOOP('',(#4170,#4171,#4172,#4173));
#731=EDGE_LOOP('',(#4174,#4175,#4176,#4177));
#732=EDGE_LOOP('',(#4178,#4179,#4180,#4181));
#733=EDGE_LOOP('',(#4182,#4183,#4184,#4185));
#734=EDGE_LOOP('',(#4186,#4187,#4188,#4189));
#735=EDGE_LOOP('',(#4190,#4191,#4192,#4193));
#736=EDGE_LOOP('',(#4194,#4195,#4196,#4197));
#737=EDGE_LOOP('',(#4198,#4199,#4200,#4201));
#738=EDGE_LOOP('',(#4202,#4203,#4204,#4205));
#739=EDGE_LOOP('',(#4206,#4207,#4208,#4209));
#740=EDGE_LOOP('',(#4210,#4211,#4212,#4213));
#741=EDGE_LOOP('',(#4214,#4215,#4216,#4217));
#742=EDGE_LOOP('',(#4218,#4219,#4220,#4221));
#743=EDGE_LOOP('',(#4222,#4223,#4224,#4225));
#744=EDGE_LOOP('',(#4226,#4227,#4228,#4229));
#745=EDGE_LOOP('',(#4230,#4231,#4232,#4233));
#746=EDGE_LOOP('',(#4234,#4235,#4236,#4237));
#747=EDGE_LOOP('',(#4238,#4239,#4240,#4241));
#748=EDGE_LOOP('',(#4242,#4243,#4244,#4245));
#749=EDGE_LOOP('',(#4246,#4247,#4248,#4249));
#750=EDGE_LOOP('',(#4250,#4251,#4252,#4253));
#751=EDGE_LOOP('',(#4254,#4255,#4256,#4257));
#752=EDGE_LOOP('',(#4258,#4259,#4260,#4261));
#753=EDGE_LOOP('',(#4262,#4263,#4264,#4265));
#754=EDGE_LOOP('',(#4266,#4267,#4268,#4269));
#755=EDGE_LOOP('',(#4270,#4271,#4272,#4273));
#756=EDGE_LOOP('',(#4274,#4275,#4276,#4277));
#757=EDGE_LOOP('',(#4278,#4279,#4280,#4281));
#758=EDGE_LOOP('',(#4282,#4283,#4284,#4285));
#759=EDGE_LOOP('',(#4286,#4287,#4288,#4289));
#760=EDGE_LOOP('',(#4290,#4291,#4292,#4293));
#761=EDGE_LOOP('',(#4294,#4295,#4296,#4297));
#762=EDGE_LOOP('',(#4298,#4299,#4300,#4301));
#763=EDGE_LOOP('',(#4302,#4303,#4304,#4305));
#764=EDGE_LOOP('',(#4306,#4307,#4308,#4309));
#765=EDGE_LOOP('',(#4310,#4311,#4312,#4313));
#766=EDGE_LOOP('',(#4314,#4315,#4316,#4317));
#767=EDGE_LOOP('',(#4318,#4319,#4320,#4321));
#768=EDGE_LOOP('',(#4322,#4323,#4324,#4325));
#769=EDGE_LOOP('',(#4326,#4327,#4328,#4329));
#770=EDGE_LOOP('',(#4330,#4331,#4332,#4333));
#771=EDGE_LOOP('',(#4334,#4335,#4336,#4337));
#772=EDGE_LOOP('',(#4338,#4339,#4340,#4341));
#773=EDGE_LOOP('',(#4342,#4343,#4344,#4345));
#774=EDGE_LOOP('',(#4346,#4347,#4348,#4349));
#775=EDGE_LOOP('',(#4350,#4351,#4352,#4353));
#776=EDGE_LOOP('',(#4354,#4355,#4356,#4357));
#777=EDGE_LOOP('',(#4358,#4359,#4360,#4361));
#778=EDGE_LOOP('',(#4362,#4363,#4364,#4365));
#779=EDGE_LOOP('',(#4366,#4367,#4368,#4369));
#780=EDGE_LOOP('',(#4370,#4371,#4372,#4373));
#781=EDGE_LOOP('',(#4374,#4375,#4376,#4377));
#782=EDGE_LOOP('',(#4378,#4379,#4380,#4381));
#783=EDGE_LOOP('',(#4382,#4383,#4384,#4385));
#784=EDGE_LOOP('',(#4386,#4387,#4388,#4389));
#785=EDGE_LOOP('',(#4390,#4391,#4392,#4393));
#786=EDGE_LOOP('',(#4394,#4395,#4396,#4397));
#787=EDGE_LOOP('',(#4398,#4399,#4400,#4401));
#788=EDGE_LOOP('',(#4402,#4403,#4404,#4405));
#789=EDGE_LOOP('',(#4406,#4407,#4408,#4409));
#790=EDGE_LOOP('',(#4410,#4411,#4412,#4413));
#791=EDGE_LOOP('',(#4414,#4415,#4416,#4417));
#792=EDGE_LOOP('',(#4418,#4419,#4420,#4421));
#793=EDGE_LOOP('',(#4422,#4423,#4424,#4425));
#794=EDGE_LOOP('',(#4426,#4427,#4428,#4429));
#795=EDGE_LOOP('',(#4430,#4431,#4432,#4433));
#796=EDGE_LOOP('',(#4434,#4435,#4436,#4437));
#797=EDGE_LOOP('',(#4438,#4439,#4440,#4441));
#798=EDGE_LOOP('',(#4442,#4443,#4444,#4445));
#799=EDGE_LOOP('',(#4446,#4447,#4448,#4449));
#800=EDGE_LOOP('',(#4450,#4451,#4452,#4453));
#801=EDGE_LOOP('',(#4454,#4455,#4456,#4457));
#802=EDGE_LOOP('',(#4458,#4459,#4460,#4461));
#803=EDGE_LOOP('',(#4462,#4463,#4464,#4465));
#804=EDGE_LOOP('',(#4466,#4467,#4468,#4469));
#805=EDGE_LOOP('',(#4470,#4471,#4472,#4473));
#806=EDGE_LOOP('',(#4474,#4475,#4476,#4477));
#807=EDGE_LOOP('',(#4478,#4479,#4480,#4481));
#808=EDGE_LOOP('',(#4482,#4483,#4484));
#809=EDGE_LOOP('',(#4485,#4486,#4487));
#810=EDGE_LOOP('',(#4488,#4489,#4490,#4491,#4492,#4493));
#811=EDGE_LOOP('',(#4494,#4495,#4496,#4497,#4498,#4499));
#812=EDGE_LOOP('',(#4500,#4501,#4502,#4503,#4504,#4505));
#813=EDGE_LOOP('',(#4506,#4507,#4508,#4509,#4510,#4511));
#814=EDGE_LOOP('',(#4512,#4513,#4514,#4515,#4516,#4517));
#815=EDGE_LOOP('',(#4518,#4519,#4520,#4521,#4522,#4523));
#816=EDGE_LOOP('',(#4524,#4525,#4526));
#817=EDGE_LOOP('',(#4527,#4528,#4529));
#818=EDGE_LOOP('',(#4530,#4531,#4532));
#819=EDGE_LOOP('',(#4533,#4534,#4535));
#820=EDGE_LOOP('',(#4536,#4537,#4538));
#821=EDGE_LOOP('',(#4539,#4540,#4541,#4542,#4543,#4544));
#822=EDGE_LOOP('',(#4545));
#823=EDGE_LOOP('',(#4546,#4547,#4548));
#824=EDGE_LOOP('',(#4549,#4550,#4551));
#825=EDGE_LOOP('',(#4552,#4553,#4554));
#826=EDGE_LOOP('',(#4555,#4556,#4557));
#827=EDGE_LOOP('',(#4558,#4559,#4560));
#828=EDGE_LOOP('',(#4561,#4562,#4563,#4564,#4565,#4566));
#829=EDGE_LOOP('',(#4567));
#830=EDGE_LOOP('',(#4568,#4569,#4570,#4571));
#831=EDGE_LOOP('',(#4572,#4573,#4574,#4575));
#832=EDGE_LOOP('',(#4576,#4577,#4578,#4579));
#833=EDGE_LOOP('',(#4580,#4581,#4582,#4583));
#834=EDGE_LOOP('',(#4584,#4585,#4586,#4587));
#835=EDGE_LOOP('',(#4588,#4589,#4590,#4591));
#836=EDGE_LOOP('',(#4592,#4593,#4594,#4595));
#837=EDGE_LOOP('',(#4596));
#838=EDGE_LOOP('',(#4597));
#839=EDGE_LOOP('',(#4598));
#840=EDGE_LOOP('',(#4599));
#841=EDGE_LOOP('',(#4600));
#842=EDGE_LOOP('',(#4601));
#843=EDGE_LOOP('',(#4602));
#844=EDGE_LOOP('',(#4603));
#845=EDGE_LOOP('',(#4604));
#846=EDGE_LOOP('',(#4605));
#847=EDGE_LOOP('',(#4606));
#848=EDGE_LOOP('',(#4607));
#849=EDGE_LOOP('',(#4608));
#850=EDGE_LOOP('',(#4609));
#851=EDGE_LOOP('',(#4610,#4611,#4612,#4613));
#852=EDGE_LOOP('',(#4614,#4615,#4616,#4617));
#853=EDGE_LOOP('',(#4618));
#854=EDGE_LOOP('',(#4619));
#855=EDGE_LOOP('',(#4620));
#856=EDGE_LOOP('',(#4621));
#857=EDGE_LOOP('',(#4622,#4623,#4624,#4625));
#858=EDGE_LOOP('',(#4626,#4627,#4628,#4629,#4630,#4631));
#859=EDGE_LOOP('',(#4632));
#860=EDGE_LOOP('',(#4633,#4634,#4635,#4636));
#861=EDGE_LOOP('',(#4637,#4638,#4639,#4640));
#862=EDGE_LOOP('',(#4641,#4642,#4643,#4644));
#863=EDGE_LOOP('',(#4645,#4646,#4647,#4648));
#864=EDGE_LOOP('',(#4649,#4650,#4651,#4652));
#865=EDGE_LOOP('',(#4653,#4654,#4655,#4656));
#866=EDGE_LOOP('',(#4657,#4658,#4659,#4660,#4661,#4662));
#867=EDGE_LOOP('',(#4663));
#868=EDGE_LOOP('',(#4664,#4665,#4666,#4667));
#869=EDGE_LOOP('',(#4668,#4669,#4670,#4671));
#870=EDGE_LOOP('',(#4672,#4673,#4674,#4675));
#871=EDGE_LOOP('',(#4676,#4677,#4678,#4679));
#872=EDGE_LOOP('',(#4680,#4681,#4682,#4683));
#873=EDGE_LOOP('',(#4684,#4685,#4686,#4687,#4688));
#874=EDGE_LOOP('',(#4689,#4690,#4691,#4692));
#875=EDGE_LOOP('',(#4693,#4694,#4695,#4696));
#876=EDGE_LOOP('',(#4697,#4698,#4699,#4700));
#877=EDGE_LOOP('',(#4701,#4702,#4703,#4704));
#878=EDGE_LOOP('',(#4705,#4706,#4707,#4708,#4709,#4710,#4711,#4712,#4713,
#4714));
#879=EDGE_LOOP('',(#4715,#4716,#4717));
#880=EDGE_LOOP('',(#4718,#4719,#4720));
#881=EDGE_LOOP('',(#4721,#4722,#4723,#4724,#4725,#4726));
#882=EDGE_LOOP('',(#4727,#4728,#4729,#4730,#4731));
#883=EDGE_LOOP('',(#4732));
#884=EDGE_LOOP('',(#4733,#4734,#4735,#4736,#4737));
#885=EDGE_LOOP('',(#4738,#4739,#4740,#4741));
#886=EDGE_LOOP('',(#4742,#4743,#4744,#4745));
#887=EDGE_LOOP('',(#4746,#4747,#4748,#4749));
#888=EDGE_LOOP('',(#4750,#4751,#4752,#4753));
#889=EDGE_LOOP('',(#4754,#4755,#4756,#4757));
#890=EDGE_LOOP('',(#4758,#4759,#4760,#4761,#4762));
#891=EDGE_LOOP('',(#4763,#4764,#4765,#4766));
#892=EDGE_LOOP('',(#4767,#4768,#4769,#4770,#4771,#4772,#4773,#4774,#4775,
#4776,#4777,#4778,#4779));
#893=EDGE_LOOP('',(#4780,#4781,#4782,#4783,#4784,#4785,#4786,#4787,#4788,
#4789,#4790,#4791,#4792,#4793));
#894=LINE('',#7955,#1185);
#895=LINE('',#7961,#1186);
#896=LINE('',#7967,#1187);
#897=LINE('',#7973,#1188);
#898=LINE('',#7979,#1189);
#899=LINE('',#7985,#1190);
#900=LINE('',#7991,#1191);
#901=LINE('',#7997,#1192);
#902=LINE('',#8003,#1193);
#903=LINE('',#8008,#1194);
#904=LINE('',#8010,#1195);
#905=LINE('',#8012,#1196);
#906=LINE('',#8013,#1197);
#907=LINE('',#8017,#1198);
#908=LINE('',#8019,#1199);
#909=LINE('',#8021,#1200);
#910=LINE('',#8022,#1201);
#911=LINE('',#8024,#1202);
#912=LINE('',#8026,#1203);
#913=LINE('',#8028,#1204);
#914=LINE('',#8029,#1205);
#915=LINE('',#8031,#1206);
#916=LINE('',#8033,#1207);
#917=LINE('',#8035,#1208);
#918=LINE('',#8036,#1209);
#919=LINE('',#8041,#1210);
#920=LINE('',#8043,#1211);
#921=LINE('',#8050,#1212);
#922=LINE('',#8057,#1213);
#923=LINE('',#8061,#1214);
#924=LINE('',#8065,#1215);
#925=LINE('',#8070,#1216);
#926=LINE('',#8080,#1217);
#927=LINE('',#8086,#1218);
#928=LINE('',#8093,#1219);
#929=LINE('',#8094,#1220);
#930=LINE('',#8097,#1221);
#931=LINE('',#8099,#1222);
#932=LINE('',#8100,#1223);
#933=LINE('',#8103,#1224);
#934=LINE('',#8104,#1225);
#935=LINE('',#8107,#1226);
#936=LINE('',#8108,#1227);
#937=LINE('',#8110,#1228);
#938=LINE('',#8119,#1229);
#939=LINE('',#8122,#1230);
#940=LINE('',#8128,#1231);
#941=LINE('',#8131,#1232);
#942=LINE('',#8136,#1233);
#943=LINE('',#8143,#1234);
#944=LINE('',#8146,#1235);
#945=LINE('',#8151,#1236);
#946=LINE('',#8158,#1237);
#947=LINE('',#8161,#1238);
#948=LINE('',#8167,#1239);
#949=LINE('',#8173,#1240);
#950=LINE('',#8176,#1241);
#951=LINE('',#8182,#1242);
#952=LINE('',#8188,#1243);
#953=LINE('',#8191,#1244);
#954=LINE('',#8197,#1245);
#955=LINE('',#8200,#1246);
#956=LINE('',#8206,#1247);
#957=LINE('',#8209,#1248);
#958=LINE('',#8215,#1249);
#959=LINE('',#8218,#1250);
#960=LINE('',#8224,#1251);
#961=LINE('',#8227,#1252);
#962=LINE('',#8233,#1253);
#963=LINE('',#8236,#1254);
#964=LINE('',#8242,#1255);
#965=LINE('',#8245,#1256);
#966=LINE('',#8251,#1257);
#967=LINE('',#8254,#1258);
#968=LINE('',#8260,#1259);
#969=LINE('',#8263,#1260);
#970=LINE('',#8269,#1261);
#971=LINE('',#8272,#1262);
#972=LINE('',#8278,#1263);
#973=LINE('',#8281,#1264);
#974=LINE('',#8287,#1265);
#975=LINE('',#8290,#1266);
#976=LINE('',#8296,#1267);
#977=LINE('',#8299,#1268);
#978=LINE('',#8305,#1269);
#979=LINE('',#8308,#1270);
#980=LINE('',#8314,#1271);
#981=LINE('',#8317,#1272);
#982=LINE('',#8323,#1273);
#983=LINE('',#8326,#1274);
#984=LINE('',#8332,#1275);
#985=LINE('',#8335,#1276);
#986=LINE('',#8341,#1277);
#987=LINE('',#8344,#1278);
#988=LINE('',#8350,#1279);
#989=LINE('',#8353,#1280);
#990=LINE('',#8359,#1281);
#991=LINE('',#8362,#1282);
#992=LINE('',#8368,#1283);
#993=LINE('',#8371,#1284);
#994=LINE('',#8377,#1285);
#995=LINE('',#8380,#1286);
#996=LINE('',#8386,#1287);
#997=LINE('',#8389,#1288);
#998=LINE('',#8395,#1289);
#999=LINE('',#8398,#1290);
#1000=LINE('',#8403,#1291);
#1001=LINE('',#8409,#1292);
#1002=LINE('',#8415,#1293);
#1003=LINE('',#8422,#1294);
#1004=LINE('',#8425,#1295);
#1005=LINE('',#8431,#1296);
#1006=LINE('',#8434,#1297);
#1007=LINE('',#8440,#1298);
#1008=LINE('',#8443,#1299);
#1009=LINE('',#8449,#1300);
#1010=LINE('',#8452,#1301);
#1011=LINE('',#8458,#1302);
#1012=LINE('',#8461,#1303);
#1013=LINE('',#8467,#1304);
#1014=LINE('',#8470,#1305);
#1015=LINE('',#8476,#1306);
#1016=LINE('',#8479,#1307);
#1017=LINE('',#8485,#1308);
#1018=LINE('',#8488,#1309);
#1019=LINE('',#8494,#1310);
#1020=LINE('',#8497,#1311);
#1021=LINE('',#8503,#1312);
#1022=LINE('',#8506,#1313);
#1023=LINE('',#8512,#1314);
#1024=LINE('',#8515,#1315);
#1025=LINE('',#8521,#1316);
#1026=LINE('',#8524,#1317);
#1027=LINE('',#8754,#1318);
#1028=LINE('',#8755,#1319);
#1029=LINE('',#8756,#1320);
#1030=LINE('',#8985,#1321);
#1031=LINE('',#8987,#1322);
#1032=LINE('',#8988,#1323);
#1033=LINE('',#8990,#1324);
#1034=LINE('',#8992,#1325);
#1035=LINE('',#8994,#1326);
#1036=LINE('',#8996,#1327);
#1037=LINE('',#8997,#1328);
#1038=LINE('',#9001,#1329);
#1039=LINE('',#9003,#1330);
#1040=LINE('',#9005,#1331);
#1041=LINE('',#9007,#1332);
#1042=LINE('',#9011,#1333);
#1043=LINE('',#9013,#1334);
#1044=LINE('',#9017,#1335);
#1045=LINE('',#9019,#1336);
#1046=LINE('',#9023,#1337);
#1047=LINE('',#9025,#1338);
#1048=LINE('',#9029,#1339);
#1049=LINE('',#9031,#1340);
#1050=LINE('',#9035,#1341);
#1051=LINE('',#9037,#1342);
#1052=LINE('',#9040,#1343);
#1053=LINE('',#9043,#1344);
#1054=LINE('',#9046,#1345);
#1055=LINE('',#9049,#1346);
#1056=LINE('',#9052,#1347);
#1057=LINE('',#9055,#1348);
#1058=LINE('',#9058,#1349);
#1059=LINE('',#9061,#1350);
#1060=LINE('',#9064,#1351);
#1061=LINE('',#9067,#1352);
#1062=LINE('',#9070,#1353);
#1063=LINE('',#9072,#1354);
#1064=LINE('',#9075,#1355);
#1065=LINE('',#9077,#1356);
#1066=LINE('',#9080,#1357);
#1067=LINE('',#9082,#1358);
#1068=LINE('',#9085,#1359);
#1069=LINE('',#9087,#1360);
#1070=LINE('',#9090,#1361);
#1071=LINE('',#9092,#1362);
#1072=LINE('',#9094,#1363);
#1073=LINE('',#9096,#1364);
#1074=LINE('',#9099,#1365);
#1075=LINE('',#9101,#1366);
#1076=LINE('',#9103,#1367);
#1077=LINE('',#9105,#1368);
#1078=LINE('',#9108,#1369);
#1079=LINE('',#9110,#1370);
#1080=LINE('',#9112,#1371);
#1081=LINE('',#9114,#1372);
#1082=LINE('',#9117,#1373);
#1083=LINE('',#9119,#1374);
#1084=LINE('',#9121,#1375);
#1085=LINE('',#9123,#1376);
#1086=LINE('',#9126,#1377);
#1087=LINE('',#9128,#1378);
#1088=LINE('',#9130,#1379);
#1089=LINE('',#9132,#1380);
#1090=LINE('',#9135,#1381);
#1091=LINE('',#9137,#1382);
#1092=LINE('',#9139,#1383);
#1093=LINE('',#9141,#1384);
#1094=LINE('',#9144,#1385);
#1095=LINE('',#9146,#1386);
#1096=LINE('',#9148,#1387);
#1097=LINE('',#9150,#1388);
#1098=LINE('',#9153,#1389);
#1099=LINE('',#9155,#1390);
#1100=LINE('',#9157,#1391);
#1101=LINE('',#9159,#1392);
#1102=LINE('',#9162,#1393);
#1103=LINE('',#9164,#1394);
#1104=LINE('',#9166,#1395);
#1105=LINE('',#9168,#1396);
#1106=LINE('',#9171,#1397);
#1107=LINE('',#9173,#1398);
#1108=LINE('',#9175,#1399);
#1109=LINE('',#9177,#1400);
#1110=LINE('',#9180,#1401);
#1111=LINE('',#9182,#1402);
#1112=LINE('',#9184,#1403);
#1113=LINE('',#9186,#1404);
#1114=LINE('',#9189,#1405);
#1115=LINE('',#9191,#1406);
#1116=LINE('',#9193,#1407);
#1117=LINE('',#9195,#1408);
#1118=LINE('',#9198,#1409);
#1119=LINE('',#9200,#1410);
#1120=LINE('',#9202,#1411);
#1121=LINE('',#9204,#1412);
#1122=LINE('',#9207,#1413);
#1123=LINE('',#9209,#1414);
#1124=LINE('',#9211,#1415);
#1125=LINE('',#9213,#1416);
#1126=LINE('',#9216,#1417);
#1127=LINE('',#9217,#1418);
#1128=LINE('',#9225,#1419);
#1129=LINE('',#9250,#1420);
#1130=LINE('',#9256,#1421);
#1131=LINE('',#9263,#1422);
#1132=LINE('',#9273,#1423);
#1133=LINE('',#9291,#1424);
#1134=LINE('',#9309,#1425);
#1135=LINE('',#9366,#1426);
#1136=LINE('',#9372,#1427);
#1137=LINE('',#9378,#1428);
#1138=LINE('',#9384,#1429);
#1139=LINE('',#9390,#1430);
#1140=LINE('',#9396,#1431);
#1141=LINE('',#9402,#1432);
#1142=LINE('',#9412,#1433);
#1143=LINE('',#9418,#1434);
#1144=LINE('',#9427,#1435);
#1145=LINE('',#9432,#1436);
#1146=LINE('',#9434,#1437);
#1147=LINE('',#9436,#1438);
#1148=LINE('',#9438,#1439);
#1149=LINE('',#9440,#1440);
#1150=LINE('',#9441,#1441);
#1151=LINE('',#9445,#1442);
#1152=LINE('',#9446,#1443);
#1153=LINE('',#9447,#1444);
#1154=LINE('',#9450,#1445);
#1155=LINE('',#9451,#1446);
#1156=LINE('',#9454,#1447);
#1157=LINE('',#9455,#1448);
#1158=LINE('',#9458,#1449);
#1159=LINE('',#9459,#1450);
#1160=LINE('',#9462,#1451);
#1161=LINE('',#9463,#1452);
#1162=LINE('',#9465,#1453);
#1163=LINE('',#9472,#1454);
#1164=LINE('',#9503,#1455);
#1165=LINE('',#9541,#1456);
#1166=LINE('',#9579,#1457);
#1167=LINE('',#9602,#1458);
#1168=LINE('',#9622,#1459);
#1169=LINE('',#9655,#1460);
#1170=LINE('',#9723,#1461);
#1171=LINE('',#9799,#1462);
#1172=LINE('',#9910,#1463);
#1173=LINE('',#9992,#1464);
#1174=LINE('',#9994,#1465);
#1175=LINE('',#9996,#1466);
#1176=LINE('',#9998,#1467);
#1177=LINE('',#10000,#1468);
#1178=LINE('',#10001,#1469);
#1179=LINE('',#10008,#1470);
#1180=LINE('',#10009,#1471);
#1181=LINE('',#10011,#1472);
#1182=LINE('',#10013,#1473);
#1183=LINE('',#10015,#1474);
#1184=LINE('',#10017,#1475);
#1185=VECTOR('',#6158,3.);
#1186=VECTOR('',#6165,3.);
#1187=VECTOR('',#6172,8.5);
#1188=VECTOR('',#6179,9.5);
#1189=VECTOR('',#6186,9.5);
#1190=VECTOR('',#6193,2.99999999999929);
#1191=VECTOR('',#6200,3.);
#1192=VECTOR('',#6207,2.99999999999976);
#1193=VECTOR('',#6214,3.);
#1194=VECTOR('',#6219,1000.);
#1195=VECTOR('',#6220,1000.);
#1196=VECTOR('',#6221,1000.);
#1197=VECTOR('',#6222,1000.);
#1198=VECTOR('',#6225,1000.);
#1199=VECTOR('',#6226,1000.);
#1200=VECTOR('',#6227,1000.);
#1201=VECTOR('',#6228,1000.);
#1202=VECTOR('',#6231,1000.);
#1203=VECTOR('',#6232,1000.);
#1204=VECTOR('',#6233,1000.);
#1205=VECTOR('',#6234,1000.);
#1206=VECTOR('',#6237,1000.);
#1207=VECTOR('',#6238,1000.);
#1208=VECTOR('',#6239,1000.);
#1209=VECTOR('',#6240,1000.);
#1210=VECTOR('',#6249,1000.);
#1211=VECTOR('',#6252,1000.);
#1212=VECTOR('',#6261,4.);
#1213=VECTOR('',#6268,1000.);
#1214=VECTOR('',#6271,4.5);
#1215=VECTOR('',#6276,1000.);
#1216=VECTOR('',#6281,5.);
#1217=VECTOR('',#6292,6.);
#1218=VECTOR('',#6299,5.);
#1219=VECTOR('',#6312,1000.);
#1220=VECTOR('',#6313,1000.);
#1221=VECTOR('',#6316,1000.);
#1222=VECTOR('',#6317,1000.);
#1223=VECTOR('',#6318,1000.);
#1224=VECTOR('',#6321,1000.);
#1225=VECTOR('',#6322,1000.);
#1226=VECTOR('',#6325,1000.);
#1227=VECTOR('',#6326,1000.);
#1228=VECTOR('',#6329,1000.);
#1229=VECTOR('',#6340,1000.);
#1230=VECTOR('',#6343,1000.);
#1231=VECTOR('',#6348,1000.);
#1232=VECTOR('',#6351,1000.);
#1233=VECTOR('',#6356,1000.);
#1234=VECTOR('',#6363,1000.);
#1235=VECTOR('',#6366,1000.);
#1236=VECTOR('',#6371,1000.);
#1237=VECTOR('',#6378,1000.);
#1238=VECTOR('',#6381,1000.);
#1239=VECTOR('',#6388,1000.);
#1240=VECTOR('',#6393,1000.);
#1241=VECTOR('',#6396,1000.);
#1242=VECTOR('',#6403,1000.);
#1243=VECTOR('',#6408,1000.);
#1244=VECTOR('',#6411,1000.);
#1245=VECTOR('',#6416,1000.);
#1246=VECTOR('',#6419,1000.);
#1247=VECTOR('',#6424,1000.);
#1248=VECTOR('',#6427,1000.);
#1249=VECTOR('',#6432,1000.);
#1250=VECTOR('',#6435,1000.);
#1251=VECTOR('',#6440,1000.);
#1252=VECTOR('',#6443,1000.);
#1253=VECTOR('',#6448,1000.);
#1254=VECTOR('',#6451,1000.);
#1255=VECTOR('',#6456,1000.);
#1256=VECTOR('',#6459,1000.);
#1257=VECTOR('',#6464,1000.);
#1258=VECTOR('',#6467,1000.);
#1259=VECTOR('',#6472,1000.);
#1260=VECTOR('',#6475,1000.);
#1261=VECTOR('',#6480,1000.);
#1262=VECTOR('',#6483,1000.);
#1263=VECTOR('',#6488,1000.);
#1264=VECTOR('',#6491,1000.);
#1265=VECTOR('',#6496,1000.);
#1266=VECTOR('',#6499,1000.);
#1267=VECTOR('',#6504,1000.);
#1268=VECTOR('',#6507,1000.);
#1269=VECTOR('',#6512,1000.);
#1270=VECTOR('',#6515,1000.);
#1271=VECTOR('',#6520,1000.);
#1272=VECTOR('',#6523,1000.);
#1273=VECTOR('',#6528,1000.);
#1274=VECTOR('',#6531,1000.);
#1275=VECTOR('',#6536,1000.);
#1276=VECTOR('',#6539,1000.);
#1277=VECTOR('',#6544,1000.);
#1278=VECTOR('',#6547,1000.);
#1279=VECTOR('',#6552,1000.);
#1280=VECTOR('',#6555,1000.);
#1281=VECTOR('',#6560,1000.);
#1282=VECTOR('',#6563,1000.);
#1283=VECTOR('',#6568,1000.);
#1284=VECTOR('',#6571,1000.);
#1285=VECTOR('',#6576,1000.);
#1286=VECTOR('',#6579,1000.);
#1287=VECTOR('',#6584,1000.);
#1288=VECTOR('',#6587,1000.);
#1289=VECTOR('',#6592,1000.);
#1290=VECTOR('',#6595,1000.);
#1291=VECTOR('',#6600,1000.);
#1292=VECTOR('',#6607,1000.);
#1293=VECTOR('',#6614,1000.);
#1294=VECTOR('',#6621,1000.);
#1295=VECTOR('',#6624,1000.);
#1296=VECTOR('',#6629,1000.);
#1297=VECTOR('',#6632,1000.);
#1298=VECTOR('',#6637,1000.);
#1299=VECTOR('',#6640,1000.);
#1300=VECTOR('',#6645,1000.);
#1301=VECTOR('',#6648,1000.);
#1302=VECTOR('',#6653,1000.);
#1303=VECTOR('',#6656,1000.);
#1304=VECTOR('',#6661,1000.);
#1305=VECTOR('',#6664,1000.);
#1306=VECTOR('',#6669,1000.);
#1307=VECTOR('',#6672,1000.);
#1308=VECTOR('',#6677,1000.);
#1309=VECTOR('',#6680,1000.);
#1310=VECTOR('',#6685,1000.);
#1311=VECTOR('',#6688,1000.);
#1312=VECTOR('',#6693,1000.);
#1313=VECTOR('',#6696,1000.);
#1314=VECTOR('',#6701,1000.);
#1315=VECTOR('',#6704,1000.);
#1316=VECTOR('',#6709,1000.);
#1317=VECTOR('',#6712,1000.);
#1318=VECTOR('',#6981,1000.);
#1319=VECTOR('',#6982,1000.);
#1320=VECTOR('',#6983,1000.);
#1321=VECTOR('',#7252,1000.);
#1322=VECTOR('',#7253,1000.);
#1323=VECTOR('',#7254,1000.);
#1324=VECTOR('',#7257,1000.);
#1325=VECTOR('',#7260,1000.);
#1326=VECTOR('',#7263,1000.);
#1327=VECTOR('',#7266,1000.);
#1328=VECTOR('',#7267,1000.);
#1329=VECTOR('',#7274,1000.);
#1330=VECTOR('',#7277,1000.);
#1331=VECTOR('',#7280,1000.);
#1332=VECTOR('',#7283,1000.);
#1333=VECTOR('',#7290,1000.);
#1334=VECTOR('',#7293,1000.);
#1335=VECTOR('',#7300,1000.);
#1336=VECTOR('',#7303,1000.);
#1337=VECTOR('',#7310,1000.);
#1338=VECTOR('',#7313,1000.);
#1339=VECTOR('',#7320,1000.);
#1340=VECTOR('',#7323,1000.);
#1341=VECTOR('',#7330,1000.);
#1342=VECTOR('',#7333,1000.);
#1343=VECTOR('',#7338,1000.);
#1344=VECTOR('',#7343,1000.);
#1345=VECTOR('',#7348,1000.);
#1346=VECTOR('',#7353,1000.);
#1347=VECTOR('',#7358,1000.);
#1348=VECTOR('',#7363,1000.);
#1349=VECTOR('',#7368,1000.);
#1350=VECTOR('',#7373,1000.);
#1351=VECTOR('',#7378,1000.);
#1352=VECTOR('',#7383,1000.);
#1353=VECTOR('',#7388,1000.);
#1354=VECTOR('',#7391,1000.);
#1355=VECTOR('',#7396,1000.);
#1356=VECTOR('',#7399,1000.);
#1357=VECTOR('',#7404,1000.);
#1358=VECTOR('',#7407,1000.);
#1359=VECTOR('',#7412,1000.);
#1360=VECTOR('',#7415,1000.);
#1361=VECTOR('',#7420,1000.);
#1362=VECTOR('',#7423,1000.);
#1363=VECTOR('',#7426,1000.);
#1364=VECTOR('',#7429,1000.);
#1365=VECTOR('',#7434,1000.);
#1366=VECTOR('',#7437,1000.);
#1367=VECTOR('',#7440,1000.);
#1368=VECTOR('',#7443,1000.);
#1369=VECTOR('',#7448,1000.);
#1370=VECTOR('',#7451,1000.);
#1371=VECTOR('',#7454,1000.);
#1372=VECTOR('',#7457,1000.);
#1373=VECTOR('',#7462,1000.);
#1374=VECTOR('',#7465,1000.);
#1375=VECTOR('',#7468,1000.);
#1376=VECTOR('',#7471,1000.);
#1377=VECTOR('',#7476,1000.);
#1378=VECTOR('',#7479,1000.);
#1379=VECTOR('',#7482,1000.);
#1380=VECTOR('',#7485,1000.);
#1381=VECTOR('',#7490,1000.);
#1382=VECTOR('',#7493,1000.);
#1383=VECTOR('',#7496,1000.);
#1384=VECTOR('',#7499,1000.);
#1385=VECTOR('',#7504,1000.);
#1386=VECTOR('',#7507,1000.);
#1387=VECTOR('',#7510,1000.);
#1388=VECTOR('',#7513,1000.);
#1389=VECTOR('',#7518,1000.);
#1390=VECTOR('',#7521,1000.);
#1391=VECTOR('',#7524,1000.);
#1392=VECTOR('',#7527,1000.);
#1393=VECTOR('',#7532,1000.);
#1394=VECTOR('',#7535,1000.);
#1395=VECTOR('',#7538,1000.);
#1396=VECTOR('',#7541,1000.);
#1397=VECTOR('',#7546,1000.);
#1398=VECTOR('',#7549,1000.);
#1399=VECTOR('',#7552,1000.);
#1400=VECTOR('',#7555,1000.);
#1401=VECTOR('',#7560,1000.);
#1402=VECTOR('',#7563,1000.);
#1403=VECTOR('',#7566,1000.);
#1404=VECTOR('',#7569,1000.);
#1405=VECTOR('',#7574,1000.);
#1406=VECTOR('',#7577,1000.);
#1407=VECTOR('',#7580,1000.);
#1408=VECTOR('',#7583,1000.);
#1409=VECTOR('',#7588,1000.);
#1410=VECTOR('',#7591,1000.);
#1411=VECTOR('',#7594,1000.);
#1412=VECTOR('',#7597,1000.);
#1413=VECTOR('',#7602,1000.);
#1414=VECTOR('',#7605,1000.);
#1415=VECTOR('',#7608,1000.);
#1416=VECTOR('',#7611,1000.);
#1417=VECTOR('',#7616,1000.);
#1418=VECTOR('',#7617,1000.);
#1419=VECTOR('',#7628,3.4);
#1420=VECTOR('',#7641,1000.);
#1421=VECTOR('',#7642,1000.);
#1422=VECTOR('',#7645,1000.);
#1423=VECTOR('',#7648,1000.);
#1424=VECTOR('',#7651,1000.);
#1425=VECTOR('',#7654,1000.);
#1426=VECTOR('',#7707,8.);
#1427=VECTOR('',#7714,25.);
#1428=VECTOR('',#7721,3.);
#1429=VECTOR('',#7728,3.);
#1430=VECTOR('',#7735,3.);
#1431=VECTOR('',#7742,3.);
#1432=VECTOR('',#7749,9.5);
#1433=VECTOR('',#7764,5.);
#1434=VECTOR('',#7771,9.5);
#1435=VECTOR('',#7784,2.5);
#1436=VECTOR('',#7789,1000.);
#1437=VECTOR('',#7790,1000.);
#1438=VECTOR('',#7791,1000.);
#1439=VECTOR('',#7792,1000.);
#1440=VECTOR('',#7793,1000.);
#1441=VECTOR('',#7794,1000.);
#1442=VECTOR('',#7797,1000.);
#1443=VECTOR('',#7798,1000.);
#1444=VECTOR('',#7799,1000.);
#1445=VECTOR('',#7802,1000.);
#1446=VECTOR('',#7803,1000.);
#1447=VECTOR('',#7806,1000.);
#1448=VECTOR('',#7807,1000.);
#1449=VECTOR('',#7810,1000.);
#1450=VECTOR('',#7811,1000.);
#1451=VECTOR('',#7814,1000.);
#1452=VECTOR('',#7815,1000.);
#1453=VECTOR('',#7818,1000.);
#1454=VECTOR('',#7827,2.54979787499999);
#1455=VECTOR('',#7832,2.54979787499999);
#1456=VECTOR('',#7835,2.54979787499999);
#1457=VECTOR('',#7838,2.54979787499999);
#1458=VECTOR('',#7843,2.008532);
#1459=VECTOR('',#7850,2.5);
#1460=VECTOR('',#7857,2.008532);
#1461=VECTOR('',#7860,2.008532);
#1462=VECTOR('',#7863,2.008532);
#1463=VECTOR('',#7868,5.06);
#1464=VECTOR('',#7881,1000.);
#1465=VECTOR('',#7882,1000.);
#1466=VECTOR('',#7883,1000.);
#1467=VECTOR('',#7884,1000.);
#1468=VECTOR('',#7885,1000.);
#1469=VECTOR('',#7886,1000.);
#1470=VECTOR('',#7899,1000.);
#1471=VECTOR('',#7900,1000.);
#1472=VECTOR('',#7903,1000.);
#1473=VECTOR('',#7906,1000.);
#1474=VECTOR('',#7909,1000.);
#1475=VECTOR('',#7912,1000.);
#1476=CIRCLE('',#5399,3.);
#1477=CIRCLE('',#5400,3.);
#1478=CIRCLE('',#5402,3.);
#1479=CIRCLE('',#5403,3.);
#1480=CIRCLE('',#5405,8.5);
#1481=CIRCLE('',#5406,8.5);
#1482=CIRCLE('',#5408,9.5);
#1483=CIRCLE('',#5409,9.5);
#1484=CIRCLE('',#5411,9.5);
#1485=CIRCLE('',#5412,9.5);
#1486=CIRCLE('',#5414,2.99999999999929);
#1487=CIRCLE('',#5415,2.99999999999929);
#1488=CIRCLE('',#5417,3.);
#1489=CIRCLE('',#5418,3.);
#1490=CIRCLE('',#5420,2.99999999999976);
#1491=CIRCLE('',#5421,2.99999999999976);
#1492=CIRCLE('',#5423,3.);
#1493=CIRCLE('',#5424,3.);
#1494=CIRCLE('',#5437,4.);
#1495=CIRCLE('',#5438,4.);
#1496=CIRCLE('',#5440,4.5);
#1497=CIRCLE('',#5441,4.5);
#1498=CIRCLE('',#5442,4.5);
#1499=CIRCLE('',#5443,4.5);
#1500=CIRCLE('',#5445,5.);
#1501=CIRCLE('',#5446,5.);
#1502=CIRCLE('',#5447,5.);
#1503=CIRCLE('',#5448,5.);
#1504=CIRCLE('',#5450,6.);
#1505=CIRCLE('',#5451,6.);
#1506=CIRCLE('',#5453,5.);
#1507=CIRCLE('',#5454,5.);
#1508=CIRCLE('',#5468,4.5);
#1509=CIRCLE('',#5469,4.5);
#1510=CIRCLE('',#5471,0.405000000000006);
#1511=CIRCLE('',#5472,0.405000000000006);
#1512=CIRCLE('',#5474,5.53127226019911);
#1513=CIRCLE('',#5475,5.53127226019911);
#1514=CIRCLE('',#5477,0.404999999999998);
#1515=CIRCLE('',#5478,0.404999999999998);
#1516=CIRCLE('',#5480,5.53127226019911);
#1517=CIRCLE('',#5481,5.53127226019914);
#1518=CIRCLE('',#5483,0.404999999999992);
#1519=CIRCLE('',#5484,0.404999999999992);
#1520=CIRCLE('',#5486,5.53127226019909);
#1521=CIRCLE('',#5487,5.5312722601991);
#1522=CIRCLE('',#5489,0.405);
#1523=CIRCLE('',#5490,0.404999999999998);
#1524=CIRCLE('',#5492,5.53127226019911);
#1525=CIRCLE('',#5493,5.53127226019911);
#1526=CIRCLE('',#5495,0.404999999999999);
#1527=CIRCLE('',#5496,0.404999999999999);
#1528=CIRCLE('',#5498,0.405000000000004);
#1529=CIRCLE('',#5499,0.405000000000003);
#1530=CIRCLE('',#5501,0.405000000000003);
#1531=CIRCLE('',#5502,0.404999999999999);
#1532=CIRCLE('',#5504,0.404999999999999);
#1533=CIRCLE('',#5505,0.404999999999999);
#1534=CIRCLE('',#5507,0.404999999999999);
#1535=CIRCLE('',#5508,0.404999999999999);
#1536=CIRCLE('',#5510,0.404999999999996);
#1537=CIRCLE('',#5511,0.404999999999996);
#1538=CIRCLE('',#5513,0.40500000000001);
#1539=CIRCLE('',#5514,0.40500000000001);
#1540=CIRCLE('',#5516,0.404999999999996);
#1541=CIRCLE('',#5517,0.405000000000001);
#1542=CIRCLE('',#5519,0.404999999999996);
#1543=CIRCLE('',#5520,0.404999999999996);
#1544=CIRCLE('',#5522,0.404999999999996);
#1545=CIRCLE('',#5523,0.404999999999996);
#1546=CIRCLE('',#5525,21.6000000000069);
#1547=CIRCLE('',#5526,21.5999999999974);
#1548=CIRCLE('',#5528,21.6000000000069);
#1549=CIRCLE('',#5529,21.6000000000079);
#1550=CIRCLE('',#5531,21.6000000000022);
#1551=CIRCLE('',#5532,21.6000000000022);
#1552=CIRCLE('',#5534,21.6000000000017);
#1553=CIRCLE('',#5535,21.6000000000017);
#1554=CIRCLE('',#5537,21.6000000000002);
#1555=CIRCLE('',#5538,21.600000000003);
#1556=CIRCLE('',#5540,21.6000000000047);
#1557=CIRCLE('',#5541,21.6000000000107);
#1558=CIRCLE('',#5543,21.6000000000067);
#1559=CIRCLE('',#5544,21.6000000000066);
#1560=CIRCLE('',#5546,21.6000000000054);
#1561=CIRCLE('',#5547,21.600000000006);
#1562=CIRCLE('',#5549,21.599999999993);
#1563=CIRCLE('',#5550,21.5999999999977);
#1564=CIRCLE('',#5552,21.6000000000103);
#1565=CIRCLE('',#5553,21.6000000000038);
#1566=CIRCLE('',#5555,21.5999999999939);
#1567=CIRCLE('',#5556,21.6000000000019);
#1568=CIRCLE('',#5558,21.6000000000017);
#1569=CIRCLE('',#5559,21.599999999998);
#1570=CIRCLE('',#5561,21.6000000000022);
#1571=CIRCLE('',#5562,21.5999999999987);
#1572=CIRCLE('',#5564,21.6000000000105);
#1573=CIRCLE('',#5565,21.6000000000104);
#1574=CIRCLE('',#5567,21.5999999999996);
#1575=CIRCLE('',#5568,21.6000000000046);
#1576=CIRCLE('',#5570,21.6000000000023);
#1577=CIRCLE('',#5571,21.5999999999979);
#1578=CIRCLE('',#5573,21.5999999999993);
#1579=CIRCLE('',#5574,21.6000000000028);
#1580=CIRCLE('',#5576,21.6000000000016);
#1581=CIRCLE('',#5577,21.6000000000009);
#1582=CIRCLE('',#5579,21.5999999999992);
#1583=CIRCLE('',#5580,21.6000000000034);
#1584=CIRCLE('',#5582,21.6000000000071);
#1585=CIRCLE('',#5583,21.6000000000056);
#1586=CIRCLE('',#5585,21.6000000000013);
#1587=CIRCLE('',#5586,21.600000000004);
#1588=CIRCLE('',#5588,21.6000000000017);
#1589=CIRCLE('',#5589,21.6000000000059);
#1590=CIRCLE('',#5591,21.5999999999972);
#1591=CIRCLE('',#5592,21.5999999999972);
#1592=CIRCLE('',#5594,21.5999999999966);
#1593=CIRCLE('',#5595,21.5999999999966);
#1594=CIRCLE('',#5597,21.599999999999);
#1595=CIRCLE('',#5598,21.6000000000073);
#1596=CIRCLE('',#5600,21.6000000000014);
#1597=CIRCLE('',#5601,21.600000000002);
#1598=CIRCLE('',#5603,21.6000000000059);
#1599=CIRCLE('',#5604,21.6000000000053);
#1600=CIRCLE('',#5606,21.6000000000022);
#1601=CIRCLE('',#5607,21.6000000000035);
#1602=CIRCLE('',#5609,21.599999999998);
#1603=CIRCLE('',#5610,21.599999999998);
#1604=CIRCLE('',#5612,5.53127226019917);
#1605=CIRCLE('',#5613,0.405000000000003);
#1606=CIRCLE('',#5614,18.5624999999987);
#1607=CIRCLE('',#5615,0.404999999999999);
#1608=CIRCLE('',#5616,5.53127226019909);
#1609=CIRCLE('',#5617,5.53127226019908);
#1610=CIRCLE('',#5618,0.404999999999999);
#1611=CIRCLE('',#5619,18.562499999997);
#1612=CIRCLE('',#5620,0.405000000000001);
#1613=CIRCLE('',#5621,5.53127226019913);
#1614=CIRCLE('',#5622,5.5312722601991);
#1615=CIRCLE('',#5623,0.405000000000003);
#1616=CIRCLE('',#5624,18.562500000001);
#1617=CIRCLE('',#5625,0.404999999999999);
#1618=CIRCLE('',#5626,5.53127226019911);
#1619=CIRCLE('',#5627,5.53127226019907);
#1620=CIRCLE('',#5628,0.404999999999999);
#1621=CIRCLE('',#5629,18.5625000000035);
#1622=CIRCLE('',#5630,0.405000000000002);
#1623=CIRCLE('',#5631,5.5312722601991);
#1624=CIRCLE('',#5632,5.53127226019912);
#1625=CIRCLE('',#5633,0.405000000000003);
#1626=CIRCLE('',#5634,18.5624999999966);
#1627=CIRCLE('',#5635,0.404999999999999);
#1628=CIRCLE('',#5636,5.53127226019916);
#1629=CIRCLE('',#5637,5.53127226019916);
#1630=CIRCLE('',#5638,0.405000000000003);
#1631=CIRCLE('',#5639,18.5625000000007);
#1632=CIRCLE('',#5640,0.404999999999999);
#1633=CIRCLE('',#5641,5.53127226019912);
#1634=CIRCLE('',#5642,5.53127226019916);
#1635=CIRCLE('',#5643,0.405000000000003);
#1636=CIRCLE('',#5644,18.5625000000044);
#1637=CIRCLE('',#5645,0.405000000000003);
#1638=CIRCLE('',#5646,5.53127226019909);
#1639=CIRCLE('',#5647,5.53127226019908);
#1640=CIRCLE('',#5648,0.40499999999999);
#1641=CIRCLE('',#5649,18.5625000000143);
#1642=CIRCLE('',#5650,0.405000000000008);
#1643=CIRCLE('',#5651,5.53127226019909);
#1644=CIRCLE('',#5652,5.53127226019913);
#1645=CIRCLE('',#5653,0.404999999999997);
#1646=CIRCLE('',#5654,18.5624999999983);
#1647=CIRCLE('',#5655,0.404999999999996);
#1648=CIRCLE('',#5656,5.53127226019912);
#1649=CIRCLE('',#5657,5.53127226019916);
#1650=CIRCLE('',#5658,0.405000000000005);
#1651=CIRCLE('',#5659,18.5625000000123);
#1652=CIRCLE('',#5660,0.404999999999998);
#1653=CIRCLE('',#5661,5.53127226019912);
#1654=CIRCLE('',#5662,5.53127226019913);
#1655=CIRCLE('',#5663,0.404999999999998);
#1656=CIRCLE('',#5664,18.5625000000065);
#1657=CIRCLE('',#5665,0.405000000000003);
#1658=CIRCLE('',#5666,5.5312722601991);
#1659=CIRCLE('',#5667,5.53127226019913);
#1660=CIRCLE('',#5668,0.404999999999999);
#1661=CIRCLE('',#5669,18.5624999999925);
#1662=CIRCLE('',#5670,0.405000000000004);
#1663=CIRCLE('',#5671,5.53127226019914);
#1664=CIRCLE('',#5672,18.5625000000053);
#1665=CIRCLE('',#5673,0.405000000000001);
#1666=CIRCLE('',#5674,5.53127226019909);
#1667=CIRCLE('',#5675,18.5625000000105);
#1668=CIRCLE('',#5676,0.405000000000001);
#1669=CIRCLE('',#5677,5.53127226019915);
#1670=CIRCLE('',#5678,5.5312722601991);
#1671=CIRCLE('',#5679,18.5624999999963);
#1672=CIRCLE('',#5680,0.405000000000004);
#1673=CIRCLE('',#5681,5.53127226019909);
#1674=CIRCLE('',#5682,5.53127226019909);
#1675=CIRCLE('',#5683,18.5625000000014);
#1676=CIRCLE('',#5684,0.404999999999999);
#1677=CIRCLE('',#5685,5.53127226019901);
#1678=CIRCLE('',#5686,5.53127226019916);
#1679=CIRCLE('',#5687,18.5625000000026);
#1680=CIRCLE('',#5688,0.404999999999999);
#1681=CIRCLE('',#5689,5.53127226019912);
#1682=CIRCLE('',#5690,5.5312722601991);
#1683=CIRCLE('',#5691,18.5625000000025);
#1684=CIRCLE('',#5692,0.405000000000001);
#1685=CIRCLE('',#5693,5.5312722601991);
#1686=CIRCLE('',#5694,5.5312722601991);
#1687=CIRCLE('',#5695,18.5625000000043);
#1688=CIRCLE('',#5696,0.404999999999999);
#1689=CIRCLE('',#5697,5.53127226019912);
#1690=CIRCLE('',#5698,5.5312722601991);
#1691=CIRCLE('',#5699,0.404999999999996);
#1692=CIRCLE('',#5700,18.5625000000115);
#1693=CIRCLE('',#5701,5.53127226019912);
#1694=CIRCLE('',#5702,5.5312722601991);
#1695=CIRCLE('',#5703,0.404999999999992);
#1696=CIRCLE('',#5704,18.5625000000082);
#1697=CIRCLE('',#5705,5.53127226019914);
#1698=CIRCLE('',#5706,5.53127226019908);
#1699=CIRCLE('',#5707,0.404999999999996);
#1700=CIRCLE('',#5708,18.562500000006);
#1701=CIRCLE('',#5709,5.53127226019906);
#1702=CIRCLE('',#5710,5.53127226019913);
#1703=CIRCLE('',#5711,0.405000000000003);
#1704=CIRCLE('',#5712,18.5624999999967);
#1705=CIRCLE('',#5713,5.53127226019909);
#1706=CIRCLE('',#5714,5.53127226019907);
#1707=CIRCLE('',#5715,0.404999999999996);
#1708=CIRCLE('',#5716,18.562499999998);
#1709=CIRCLE('',#5717,5.53127226019909);
#1710=CIRCLE('',#5718,5.53127226019907);
#1711=CIRCLE('',#5719,0.405000000000003);
#1712=CIRCLE('',#5720,18.562500000011);
#1713=CIRCLE('',#5721,5.53127226019915);
#1714=CIRCLE('',#5722,0.405000000000003);
#1715=CIRCLE('',#5723,18.5624999999985);
#1716=CIRCLE('',#5724,21.6000000000043);
#1717=CIRCLE('',#5725,5.53127226019911);
#1718=CIRCLE('',#5726,0.405000000000002);
#1719=CIRCLE('',#5727,18.5625000000073);
#1720=CIRCLE('',#5728,0.404999999999998);
#1721=CIRCLE('',#5729,5.53127226019908);
#1722=CIRCLE('',#5730,5.53127226019911);
#1723=CIRCLE('',#5731,0.404999999999997);
#1724=CIRCLE('',#5732,18.5625000000057);
#1725=CIRCLE('',#5733,0.404999999999998);
#1726=CIRCLE('',#5734,5.53127226019911);
#1727=CIRCLE('',#5735,5.53127226019913);
#1728=CIRCLE('',#5736,0.405000000000003);
#1729=CIRCLE('',#5737,18.56250000001);
#1730=CIRCLE('',#5738,0.404999999999992);
#1731=CIRCLE('',#5739,5.53127226019908);
#1732=CIRCLE('',#5740,5.53127226019912);
#1733=CIRCLE('',#5741,0.404999999999997);
#1734=CIRCLE('',#5742,18.562500000001);
#1735=CIRCLE('',#5743,0.404999999999997);
#1736=CIRCLE('',#5744,5.5312722601991);
#1737=CIRCLE('',#5746,5.53127226019912);
#1738=CIRCLE('',#5747,5.53127226019911);
#1739=CIRCLE('',#5748,0.404999999999996);
#1740=CIRCLE('',#5749,18.562500000001);
#1741=CIRCLE('',#5750,0.405000000000003);
#1742=CIRCLE('',#5751,5.53127226019912);
#1743=CIRCLE('',#5752,5.53127226019908);
#1744=CIRCLE('',#5753,0.404999999999999);
#1745=CIRCLE('',#5754,18.56250000001);
#1746=CIRCLE('',#5755,0.405000000000004);
#1747=CIRCLE('',#5756,5.53127226019912);
#1748=CIRCLE('',#5757,5.5312722601991);
#1749=CIRCLE('',#5758,0.404999999999997);
#1750=CIRCLE('',#5759,18.5625000000057);
#1751=CIRCLE('',#5760,0.404999999999997);
#1752=CIRCLE('',#5761,5.53127226019915);
#1753=CIRCLE('',#5762,5.53127226019911);
#1754=CIRCLE('',#5763,0.404999999999998);
#1755=CIRCLE('',#5764,18.5625000000073);
#1756=CIRCLE('',#5765,0.405000000000002);
#1757=CIRCLE('',#5766,5.5312722601991);
#1758=CIRCLE('',#5767,21.5999999999959);
#1759=CIRCLE('',#5768,18.5624999999985);
#1760=CIRCLE('',#5769,0.405000000000003);
#1761=CIRCLE('',#5770,5.53127226019911);
#1762=CIRCLE('',#5771,18.562500000011);
#1763=CIRCLE('',#5772,0.405000000000003);
#1764=CIRCLE('',#5773,5.53127226019907);
#1765=CIRCLE('',#5774,5.53127226019914);
#1766=CIRCLE('',#5775,18.562499999998);
#1767=CIRCLE('',#5776,0.404999999999996);
#1768=CIRCLE('',#5777,5.53127226019908);
#1769=CIRCLE('',#5778,5.53127226019909);
#1770=CIRCLE('',#5779,18.5624999999967);
#1771=CIRCLE('',#5780,0.405000000000003);
#1772=CIRCLE('',#5781,5.53127226019919);
#1773=CIRCLE('',#5782,5.53127226019911);
#1774=CIRCLE('',#5783,18.562500000006);
#1775=CIRCLE('',#5784,0.404999999999996);
#1776=CIRCLE('',#5785,5.53127226019911);
#1777=CIRCLE('',#5786,5.53127226019915);
#1778=CIRCLE('',#5787,18.5625000000082);
#1779=CIRCLE('',#5788,0.404999999999992);
#1780=CIRCLE('',#5789,5.53127226019912);
#1781=CIRCLE('',#5790,5.53127226019915);
#1782=CIRCLE('',#5791,18.5625000000115);
#1783=CIRCLE('',#5792,0.404999999999996);
#1784=CIRCLE('',#5793,5.53127226019913);
#1785=CIRCLE('',#5794,5.53127226019912);
#1786=CIRCLE('',#5795,0.404999999999999);
#1787=CIRCLE('',#5796,18.5625000000043);
#1788=CIRCLE('',#5797,5.5312722601991);
#1789=CIRCLE('',#5798,5.53127226019909);
#1790=CIRCLE('',#5799,0.405000000000003);
#1791=CIRCLE('',#5800,18.5625000000025);
#1792=CIRCLE('',#5801,5.5312722601991);
#1793=CIRCLE('',#5802,5.53127226019911);
#1794=CIRCLE('',#5803,0.405000000000004);
#1795=CIRCLE('',#5804,18.5625000000026);
#1796=CIRCLE('',#5805,5.53127226019917);
#1797=CIRCLE('',#5806,5.5312722601991);
#1798=CIRCLE('',#5807,0.405000000000001);
#1799=CIRCLE('',#5808,18.5625000000014);
#1800=CIRCLE('',#5809,5.53127226019908);
#1801=CIRCLE('',#5810,5.53127226019907);
#1802=CIRCLE('',#5811,0.405000000000004);
#1803=CIRCLE('',#5812,18.5624999999963);
#1804=CIRCLE('',#5813,5.53127226019908);
#1805=CIRCLE('',#5814,5.53127226019914);
#1806=CIRCLE('',#5815,0.405000000000001);
#1807=CIRCLE('',#5816,18.5625000000105);
#1808=CIRCLE('',#5817,5.53127226019909);
#1809=CIRCLE('',#5818,0.404999999999999);
#1810=CIRCLE('',#5819,18.5625000000053);
#1811=CIRCLE('',#5820,5.53127226019914);
#1812=CIRCLE('',#5821,0.405);
#1813=CIRCLE('',#5822,18.5624999999925);
#1814=CIRCLE('',#5823,0.405000000000001);
#1815=CIRCLE('',#5824,5.53127226019911);
#1816=CIRCLE('',#5825,5.53127226019916);
#1817=CIRCLE('',#5826,0.405000000000002);
#1818=CIRCLE('',#5827,18.5625000000065);
#1819=CIRCLE('',#5828,0.404999999999998);
#1820=CIRCLE('',#5829,5.53127226019912);
#1821=CIRCLE('',#5830,5.53127226019915);
#1822=CIRCLE('',#5831,0.404999999999998);
#1823=CIRCLE('',#5832,18.5625000000123);
#1824=CIRCLE('',#5833,0.405000000000006);
#1825=CIRCLE('',#5834,5.53127226019916);
#1826=CIRCLE('',#5835,5.53127226019912);
#1827=CIRCLE('',#5836,0.404999999999996);
#1828=CIRCLE('',#5837,18.5624999999983);
#1829=CIRCLE('',#5838,0.404999999999997);
#1830=CIRCLE('',#5839,5.53127226019917);
#1831=CIRCLE('',#5840,5.53127226019916);
#1832=CIRCLE('',#5841,0.405000000000008);
#1833=CIRCLE('',#5842,18.5625000000143);
#1834=CIRCLE('',#5843,0.404999999999994);
#1835=CIRCLE('',#5844,5.53127226019913);
#1836=CIRCLE('',#5845,5.53127226019921);
#1837=CIRCLE('',#5846,0.404999999999999);
#1838=CIRCLE('',#5847,18.5625000000044);
#1839=CIRCLE('',#5848,0.405000000000003);
#1840=CIRCLE('',#5849,5.5312722601991);
#1841=CIRCLE('',#5850,5.53127226019908);
#1842=CIRCLE('',#5851,0.404999999999999);
#1843=CIRCLE('',#5852,18.5625000000007);
#1844=CIRCLE('',#5853,0.405000000000003);
#1845=CIRCLE('',#5854,5.53127226019911);
#1846=CIRCLE('',#5855,5.53127226019911);
#1847=CIRCLE('',#5856,0.404999999999999);
#1848=CIRCLE('',#5857,18.5624999999966);
#1849=CIRCLE('',#5858,0.405000000000003);
#1850=CIRCLE('',#5859,5.53127226019913);
#1851=CIRCLE('',#5860,5.5312722601991);
#1852=CIRCLE('',#5861,0.405000000000002);
#1853=CIRCLE('',#5862,18.5625000000035);
#1854=CIRCLE('',#5863,0.404999999999999);
#1855=CIRCLE('',#5864,5.5312722601991);
#1856=CIRCLE('',#5865,5.53127226019911);
#1857=CIRCLE('',#5866,0.404999999999999);
#1858=CIRCLE('',#5867,18.562500000001);
#1859=CIRCLE('',#5868,0.405000000000003);
#1860=CIRCLE('',#5869,5.53127226019909);
#1861=CIRCLE('',#5870,5.53127226019911);
#1862=CIRCLE('',#5871,0.405000000000001);
#1863=CIRCLE('',#5872,18.562499999997);
#1864=CIRCLE('',#5873,0.405000000000003);
#1865=CIRCLE('',#5874,5.5312722601991);
#1866=CIRCLE('',#5875,5.53127226019909);
#1867=CIRCLE('',#5876,0.404999999999999);
#1868=CIRCLE('',#5877,18.5624999999987);
#1869=CIRCLE('',#5878,0.404999999999999);
#1870=CIRCLE('',#6017,3.4);
#1871=CIRCLE('',#6018,3.4);
#1872=CIRCLE('',#6020,6.5);
#1873=CIRCLE('',#6022,6.5);
#1874=CIRCLE('',#6030,6.5);
#1875=CIRCLE('',#6032,6.5);
#1876=CIRCLE('',#6034,6.5);
#1877=CIRCLE('',#6036,6.5);
#1878=CIRCLE('',#6038,6.5);
#1879=CIRCLE('',#6041,6.5);
#1880=CIRCLE('',#6043,6.5);
#1881=CIRCLE('',#6045,6.5);
#1882=CIRCLE('',#6047,6.5);
#1883=CIRCLE('',#6049,6.5);
#1884=CIRCLE('',#6053,8.);
#1885=CIRCLE('',#6054,8.);
#1886=CIRCLE('',#6056,25.);
#1887=CIRCLE('',#6057,25.);
#1888=CIRCLE('',#6059,3.);
#1889=CIRCLE('',#6060,3.);
#1890=CIRCLE('',#6062,3.);
#1891=CIRCLE('',#6063,3.);
#1892=CIRCLE('',#6065,3.);
#1893=CIRCLE('',#6066,3.);
#1894=CIRCLE('',#6068,3.);
#1895=CIRCLE('',#6069,3.);
#1896=CIRCLE('',#6071,9.5);
#1897=CIRCLE('',#6072,9.5);
#1898=CIRCLE('',#6078,5.);
#1899=CIRCLE('',#6079,5.);
#1900=CIRCLE('',#6081,9.5);
#1901=CIRCLE('',#6082,9.5);
#1902=CIRCLE('',#6087,2.5);
#1903=CIRCLE('',#6088,2.5);
#1904=CIRCLE('',#6100,2.54979787499999);
#1905=CIRCLE('',#6104,2.54979787499999);
#1906=CIRCLE('',#6106,2.008532);
#1907=CIRCLE('',#6107,2.5);
#1908=CIRCLE('',#6109,2.008532);
#1909=CIRCLE('',#6110,2.5);
#1910=CIRCLE('',#6116,3.22);
#1911=CIRCLE('',#6118,2.5);
#1912=CIRCLE('',#6120,2.5);
#1913=CIRCLE('',#6122,2.54924752923115);
#1914=CIRCLE('',#6123,2.5195932879569);
#1915=CIRCLE('',#6125,2.54909484356462);
#1916=CIRCLE('',#6126,2.5196046498842);
#1917=VERTEX_POINT('',#7952);
#1918=VERTEX_POINT('',#7954);
#1919=VERTEX_POINT('',#7958);
#1920=VERTEX_POINT('',#7960);
#1921=VERTEX_POINT('',#7964);
#1922=VERTEX_POINT('',#7966);
#1923=VERTEX_POINT('',#7970);
#1924=VERTEX_POINT('',#7972);
#1925=VERTEX_POINT('',#7976);
#1926=VERTEX_POINT('',#7978);
#1927=VERTEX_POINT('',#7982);
#1928=VERTEX_POINT('',#7984);
#1929=VERTEX_POINT('',#7988);
#1930=VERTEX_POINT('',#7990);
#1931=VERTEX_POINT('',#7994);
#1932=VERTEX_POINT('',#7996);
#1933=VERTEX_POINT('',#8000);
#1934=VERTEX_POINT('',#8002);
#1935=VERTEX_POINT('',#8006);
#1936=VERTEX_POINT('',#8007);
#1937=VERTEX_POINT('',#8009);
#1938=VERTEX_POINT('',#8011);
#1939=VERTEX_POINT('',#8015);
#1940=VERTEX_POINT('',#8016);
#1941=VERTEX_POINT('',#8018);
#1942=VERTEX_POINT('',#8020);
#1943=VERTEX_POINT('',#8025);
#1944=VERTEX_POINT('',#8027);
#1945=VERTEX_POINT('',#8032);
#1946=VERTEX_POINT('',#8034);
#1947=VERTEX_POINT('',#8047);
#1948=VERTEX_POINT('',#8049);
#1949=VERTEX_POINT('',#8053);
#1950=VERTEX_POINT('',#8054);
#1951=VERTEX_POINT('',#8056);
#1952=VERTEX_POINT('',#8058);
#1953=VERTEX_POINT('',#8060);
#1954=VERTEX_POINT('',#8063);
#1955=VERTEX_POINT('',#8067);
#1956=VERTEX_POINT('',#8069);
#1957=VERTEX_POINT('',#8071);
#1958=VERTEX_POINT('',#8073);
#1959=VERTEX_POINT('',#8077);
#1960=VERTEX_POINT('',#8079);
#1961=VERTEX_POINT('',#8083);
#1962=VERTEX_POINT('',#8085);
#1963=VERTEX_POINT('',#8096);
#1964=VERTEX_POINT('',#8098);
#1965=VERTEX_POINT('',#8102);
#1966=VERTEX_POINT('',#8106);
#1967=VERTEX_POINT('',#8115);
#1968=VERTEX_POINT('',#8116);
#1969=VERTEX_POINT('',#8118);
#1970=VERTEX_POINT('',#8120);
#1971=VERTEX_POINT('',#8124);
#1972=VERTEX_POINT('',#8125);
#1973=VERTEX_POINT('',#8127);
#1974=VERTEX_POINT('',#8129);
#1975=VERTEX_POINT('',#8133);
#1976=VERTEX_POINT('',#8135);
#1977=VERTEX_POINT('',#8139);
#1978=VERTEX_POINT('',#8140);
#1979=VERTEX_POINT('',#8142);
#1980=VERTEX_POINT('',#8144);
#1981=VERTEX_POINT('',#8148);
#1982=VERTEX_POINT('',#8150);
#1983=VERTEX_POINT('',#8154);
#1984=VERTEX_POINT('',#8155);
#1985=VERTEX_POINT('',#8157);
#1986=VERTEX_POINT('',#8159);
#1987=VERTEX_POINT('',#8163);
#1988=VERTEX_POINT('',#8165);
#1989=VERTEX_POINT('',#8169);
#1990=VERTEX_POINT('',#8170);
#1991=VERTEX_POINT('',#8172);
#1992=VERTEX_POINT('',#8174);
#1993=VERTEX_POINT('',#8178);
#1994=VERTEX_POINT('',#8180);
#1995=VERTEX_POINT('',#8184);
#1996=VERTEX_POINT('',#8185);
#1997=VERTEX_POINT('',#8187);
#1998=VERTEX_POINT('',#8189);
#1999=VERTEX_POINT('',#8193);
#2000=VERTEX_POINT('',#8194);
#2001=VERTEX_POINT('',#8196);
#2002=VERTEX_POINT('',#8198);
#2003=VERTEX_POINT('',#8202);
#2004=VERTEX_POINT('',#8203);
#2005=VERTEX_POINT('',#8205);
#2006=VERTEX_POINT('',#8207);
#2007=VERTEX_POINT('',#8211);
#2008=VERTEX_POINT('',#8212);
#2009=VERTEX_POINT('',#8214);
#2010=VERTEX_POINT('',#8216);
#2011=VERTEX_POINT('',#8220);
#2012=VERTEX_POINT('',#8221);
#2013=VERTEX_POINT('',#8223);
#2014=VERTEX_POINT('',#8225);
#2015=VERTEX_POINT('',#8229);
#2016=VERTEX_POINT('',#8230);
#2017=VERTEX_POINT('',#8232);
#2018=VERTEX_POINT('',#8234);
#2019=VERTEX_POINT('',#8238);
#2020=VERTEX_POINT('',#8239);
#2021=VERTEX_POINT('',#8241);
#2022=VERTEX_POINT('',#8243);
#2023=VERTEX_POINT('',#8247);
#2024=VERTEX_POINT('',#8248);
#2025=VERTEX_POINT('',#8250);
#2026=VERTEX_POINT('',#8252);
#2027=VERTEX_POINT('',#8256);
#2028=VERTEX_POINT('',#8257);
#2029=VERTEX_POINT('',#8259);
#2030=VERTEX_POINT('',#8261);
#2031=VERTEX_POINT('',#8265);
#2032=VERTEX_POINT('',#8266);
#2033=VERTEX_POINT('',#8268);
#2034=VERTEX_POINT('',#8270);
#2035=VERTEX_POINT('',#8274);
#2036=VERTEX_POINT('',#8275);
#2037=VERTEX_POINT('',#8277);
#2038=VERTEX_POINT('',#8279);
#2039=VERTEX_POINT('',#8283);
#2040=VERTEX_POINT('',#8284);
#2041=VERTEX_POINT('',#8286);
#2042=VERTEX_POINT('',#8288);
#2043=VERTEX_POINT('',#8292);
#2044=VERTEX_POINT('',#8293);
#2045=VERTEX_POINT('',#8295);
#2046=VERTEX_POINT('',#8297);
#2047=VERTEX_POINT('',#8301);
#2048=VERTEX_POINT('',#8302);
#2049=VERTEX_POINT('',#8304);
#2050=VERTEX_POINT('',#8306);
#2051=VERTEX_POINT('',#8310);
#2052=VERTEX_POINT('',#8311);
#2053=VERTEX_POINT('',#8313);
#2054=VERTEX_POINT('',#8315);
#2055=VERTEX_POINT('',#8319);
#2056=VERTEX_POINT('',#8320);
#2057=VERTEX_POINT('',#8322);
#2058=VERTEX_POINT('',#8324);
#2059=VERTEX_POINT('',#8328);
#2060=VERTEX_POINT('',#8329);
#2061=VERTEX_POINT('',#8331);
#2062=VERTEX_POINT('',#8333);
#2063=VERTEX_POINT('',#8337);
#2064=VERTEX_POINT('',#8338);
#2065=VERTEX_POINT('',#8340);
#2066=VERTEX_POINT('',#8342);
#2067=VERTEX_POINT('',#8346);
#2068=VERTEX_POINT('',#8347);
#2069=VERTEX_POINT('',#8349);
#2070=VERTEX_POINT('',#8351);
#2071=VERTEX_POINT('',#8355);
#2072=VERTEX_POINT('',#8356);
#2073=VERTEX_POINT('',#8358);
#2074=VERTEX_POINT('',#8360);
#2075=VERTEX_POINT('',#8364);
#2076=VERTEX_POINT('',#8365);
#2077=VERTEX_POINT('',#8367);
#2078=VERTEX_POINT('',#8369);
#2079=VERTEX_POINT('',#8373);
#2080=VERTEX_POINT('',#8374);
#2081=VERTEX_POINT('',#8376);
#2082=VERTEX_POINT('',#8378);
#2083=VERTEX_POINT('',#8382);
#2084=VERTEX_POINT('',#8383);
#2085=VERTEX_POINT('',#8385);
#2086=VERTEX_POINT('',#8387);
#2087=VERTEX_POINT('',#8391);
#2088=VERTEX_POINT('',#8392);
#2089=VERTEX_POINT('',#8394);
#2090=VERTEX_POINT('',#8396);
#2091=VERTEX_POINT('',#8400);
#2092=VERTEX_POINT('',#8402);
#2093=VERTEX_POINT('',#8406);
#2094=VERTEX_POINT('',#8408);
#2095=VERTEX_POINT('',#8412);
#2096=VERTEX_POINT('',#8414);
#2097=VERTEX_POINT('',#8418);
#2098=VERTEX_POINT('',#8419);
#2099=VERTEX_POINT('',#8421);
#2100=VERTEX_POINT('',#8423);
#2101=VERTEX_POINT('',#8427);
#2102=VERTEX_POINT('',#8428);
#2103=VERTEX_POINT('',#8430);
#2104=VERTEX_POINT('',#8432);
#2105=VERTEX_POINT('',#8436);
#2106=VERTEX_POINT('',#8437);
#2107=VERTEX_POINT('',#8439);
#2108=VERTEX_POINT('',#8441);
#2109=VERTEX_POINT('',#8445);
#2110=VERTEX_POINT('',#8446);
#2111=VERTEX_POINT('',#8448);
#2112=VERTEX_POINT('',#8450);
#2113=VERTEX_POINT('',#8454);
#2114=VERTEX_POINT('',#8455);
#2115=VERTEX_POINT('',#8457);
#2116=VERTEX_POINT('',#8459);
#2117=VERTEX_POINT('',#8463);
#2118=VERTEX_POINT('',#8464);
#2119=VERTEX_POINT('',#8466);
#2120=VERTEX_POINT('',#8468);
#2121=VERTEX_POINT('',#8472);
#2122=VERTEX_POINT('',#8473);
#2123=VERTEX_POINT('',#8475);
#2124=VERTEX_POINT('',#8477);
#2125=VERTEX_POINT('',#8481);
#2126=VERTEX_POINT('',#8482);
#2127=VERTEX_POINT('',#8484);
#2128=VERTEX_POINT('',#8486);
#2129=VERTEX_POINT('',#8490);
#2130=VERTEX_POINT('',#8491);
#2131=VERTEX_POINT('',#8493);
#2132=VERTEX_POINT('',#8495);
#2133=VERTEX_POINT('',#8499);
#2134=VERTEX_POINT('',#8500);
#2135=VERTEX_POINT('',#8502);
#2136=VERTEX_POINT('',#8504);
#2137=VERTEX_POINT('',#8508);
#2138=VERTEX_POINT('',#8509);
#2139=VERTEX_POINT('',#8511);
#2140=VERTEX_POINT('',#8513);
#2141=VERTEX_POINT('',#8517);
#2142=VERTEX_POINT('',#8518);
#2143=VERTEX_POINT('',#8520);
#2144=VERTEX_POINT('',#8522);
#2145=VERTEX_POINT('',#8526);
#2146=VERTEX_POINT('',#8528);
#2147=VERTEX_POINT('',#8530);
#2148=VERTEX_POINT('',#8532);
#2149=VERTEX_POINT('',#8535);
#2150=VERTEX_POINT('',#8537);
#2151=VERTEX_POINT('',#8539);
#2152=VERTEX_POINT('',#8541);
#2153=VERTEX_POINT('',#8544);
#2154=VERTEX_POINT('',#8546);
#2155=VERTEX_POINT('',#8548);
#2156=VERTEX_POINT('',#8550);
#2157=VERTEX_POINT('',#8553);
#2158=VERTEX_POINT('',#8555);
#2159=VERTEX_POINT('',#8557);
#2160=VERTEX_POINT('',#8559);
#2161=VERTEX_POINT('',#8562);
#2162=VERTEX_POINT('',#8564);
#2163=VERTEX_POINT('',#8566);
#2164=VERTEX_POINT('',#8568);
#2165=VERTEX_POINT('',#8571);
#2166=VERTEX_POINT('',#8573);
#2167=VERTEX_POINT('',#8575);
#2168=VERTEX_POINT('',#8577);
#2169=VERTEX_POINT('',#8580);
#2170=VERTEX_POINT('',#8582);
#2171=VERTEX_POINT('',#8584);
#2172=VERTEX_POINT('',#8586);
#2173=VERTEX_POINT('',#8589);
#2174=VERTEX_POINT('',#8591);
#2175=VERTEX_POINT('',#8593);
#2176=VERTEX_POINT('',#8595);
#2177=VERTEX_POINT('',#8598);
#2178=VERTEX_POINT('',#8600);
#2179=VERTEX_POINT('',#8602);
#2180=VERTEX_POINT('',#8604);
#2181=VERTEX_POINT('',#8607);
#2182=VERTEX_POINT('',#8609);
#2183=VERTEX_POINT('',#8611);
#2184=VERTEX_POINT('',#8613);
#2185=VERTEX_POINT('',#8616);
#2186=VERTEX_POINT('',#8618);
#2187=VERTEX_POINT('',#8620);
#2188=VERTEX_POINT('',#8622);
#2189=VERTEX_POINT('',#8625);
#2190=VERTEX_POINT('',#8627);
#2191=VERTEX_POINT('',#8629);
#2192=VERTEX_POINT('',#8631);
#2193=VERTEX_POINT('',#8634);
#2194=VERTEX_POINT('',#8636);
#2195=VERTEX_POINT('',#8639);
#2196=VERTEX_POINT('',#8641);
#2197=VERTEX_POINT('',#8645);
#2198=VERTEX_POINT('',#8647);
#2199=VERTEX_POINT('',#8651);
#2200=VERTEX_POINT('',#8653);
#2201=VERTEX_POINT('',#8657);
#2202=VERTEX_POINT('',#8659);
#2203=VERTEX_POINT('',#8663);
#2204=VERTEX_POINT('',#8665);
#2205=VERTEX_POINT('',#8669);
#2206=VERTEX_POINT('',#8671);
#2207=VERTEX_POINT('',#8674);
#2208=VERTEX_POINT('',#8676);
#2209=VERTEX_POINT('',#8680);
#2210=VERTEX_POINT('',#8682);
#2211=VERTEX_POINT('',#8686);
#2212=VERTEX_POINT('',#8688);
#2213=VERTEX_POINT('',#8692);
#2214=VERTEX_POINT('',#8694);
#2215=VERTEX_POINT('',#8698);
#2216=VERTEX_POINT('',#8700);
#2217=VERTEX_POINT('',#8704);
#2218=VERTEX_POINT('',#8706);
#2219=VERTEX_POINT('',#8709);
#2220=VERTEX_POINT('',#8711);
#2221=VERTEX_POINT('',#8714);
#2222=VERTEX_POINT('',#8716);
#2223=VERTEX_POINT('',#8718);
#2224=VERTEX_POINT('',#8720);
#2225=VERTEX_POINT('',#8722);
#2226=VERTEX_POINT('',#8725);
#2227=VERTEX_POINT('',#8727);
#2228=VERTEX_POINT('',#8729);
#2229=VERTEX_POINT('',#8731);
#2230=VERTEX_POINT('',#8734);
#2231=VERTEX_POINT('',#8736);
#2232=VERTEX_POINT('',#8738);
#2233=VERTEX_POINT('',#8740);
#2234=VERTEX_POINT('',#8743);
#2235=VERTEX_POINT('',#8745);
#2236=VERTEX_POINT('',#8747);
#2237=VERTEX_POINT('',#8749);
#2238=VERTEX_POINT('',#8752);
#2239=VERTEX_POINT('',#8753);
#2240=VERTEX_POINT('',#8758);
#2241=VERTEX_POINT('',#8760);
#2242=VERTEX_POINT('',#8762);
#2243=VERTEX_POINT('',#8764);
#2244=VERTEX_POINT('',#8766);
#2245=VERTEX_POINT('',#8769);
#2246=VERTEX_POINT('',#8771);
#2247=VERTEX_POINT('',#8773);
#2248=VERTEX_POINT('',#8775);
#2249=VERTEX_POINT('',#8778);
#2250=VERTEX_POINT('',#8780);
#2251=VERTEX_POINT('',#8782);
#2252=VERTEX_POINT('',#8784);
#2253=VERTEX_POINT('',#8787);
#2254=VERTEX_POINT('',#8789);
#2255=VERTEX_POINT('',#8791);
#2256=VERTEX_POINT('',#8793);
#2257=VERTEX_POINT('',#8795);
#2258=VERTEX_POINT('',#8798);
#2259=VERTEX_POINT('',#8800);
#2260=VERTEX_POINT('',#8803);
#2261=VERTEX_POINT('',#8805);
#2262=VERTEX_POINT('',#8809);
#2263=VERTEX_POINT('',#8811);
#2264=VERTEX_POINT('',#8815);
#2265=VERTEX_POINT('',#8817);
#2266=VERTEX_POINT('',#8821);
#2267=VERTEX_POINT('',#8823);
#2268=VERTEX_POINT('',#8827);
#2269=VERTEX_POINT('',#8829);
#2270=VERTEX_POINT('',#8833);
#2271=VERTEX_POINT('',#8835);
#2272=VERTEX_POINT('',#8838);
#2273=VERTEX_POINT('',#8840);
#2274=VERTEX_POINT('',#8844);
#2275=VERTEX_POINT('',#8846);
#2276=VERTEX_POINT('',#8850);
#2277=VERTEX_POINT('',#8852);
#2278=VERTEX_POINT('',#8856);
#2279=VERTEX_POINT('',#8858);
#2280=VERTEX_POINT('',#8862);
#2281=VERTEX_POINT('',#8864);
#2282=VERTEX_POINT('',#8868);
#2283=VERTEX_POINT('',#8870);
#2284=VERTEX_POINT('',#8873);
#2285=VERTEX_POINT('',#8875);
#2286=VERTEX_POINT('',#8878);
#2287=VERTEX_POINT('',#8880);
#2288=VERTEX_POINT('',#8882);
#2289=VERTEX_POINT('',#8884);
#2290=VERTEX_POINT('',#8887);
#2291=VERTEX_POINT('',#8889);
#2292=VERTEX_POINT('',#8891);
#2293=VERTEX_POINT('',#8893);
#2294=VERTEX_POINT('',#8896);
#2295=VERTEX_POINT('',#8898);
#2296=VERTEX_POINT('',#8900);
#2297=VERTEX_POINT('',#8902);
#2298=VERTEX_POINT('',#8905);
#2299=VERTEX_POINT('',#8907);
#2300=VERTEX_POINT('',#8909);
#2301=VERTEX_POINT('',#8911);
#2302=VERTEX_POINT('',#8914);
#2303=VERTEX_POINT('',#8916);
#2304=VERTEX_POINT('',#8918);
#2305=VERTEX_POINT('',#8920);
#2306=VERTEX_POINT('',#8923);
#2307=VERTEX_POINT('',#8925);
#2308=VERTEX_POINT('',#8927);
#2309=VERTEX_POINT('',#8929);
#2310=VERTEX_POINT('',#8932);
#2311=VERTEX_POINT('',#8934);
#2312=VERTEX_POINT('',#8936);
#2313=VERTEX_POINT('',#8938);
#2314=VERTEX_POINT('',#8941);
#2315=VERTEX_POINT('',#8943);
#2316=VERTEX_POINT('',#8945);
#2317=VERTEX_POINT('',#8947);
#2318=VERTEX_POINT('',#8950);
#2319=VERTEX_POINT('',#8952);
#2320=VERTEX_POINT('',#8954);
#2321=VERTEX_POINT('',#8956);
#2322=VERTEX_POINT('',#8959);
#2323=VERTEX_POINT('',#8961);
#2324=VERTEX_POINT('',#8963);
#2325=VERTEX_POINT('',#8965);
#2326=VERTEX_POINT('',#8968);
#2327=VERTEX_POINT('',#8970);
#2328=VERTEX_POINT('',#8972);
#2329=VERTEX_POINT('',#8974);
#2330=VERTEX_POINT('',#8977);
#2331=VERTEX_POINT('',#8979);
#2332=VERTEX_POINT('',#8981);
#2333=VERTEX_POINT('',#8984);
#2334=VERTEX_POINT('',#8986);
#2335=VERTEX_POINT('',#9222);
#2336=VERTEX_POINT('',#9224);
#2337=VERTEX_POINT('',#9228);
#2338=VERTEX_POINT('',#9229);
#2339=VERTEX_POINT('',#9231);
#2340=VERTEX_POINT('',#9239);
#2341=VERTEX_POINT('',#9240);
#2342=VERTEX_POINT('',#9242);
#2343=VERTEX_POINT('',#9251);
#2344=VERTEX_POINT('',#9255);
#2345=VERTEX_POINT('',#9261);
#2346=VERTEX_POINT('',#9262);
#2347=VERTEX_POINT('',#9271);
#2348=VERTEX_POINT('',#9272);
#2349=VERTEX_POINT('',#9274);
#2350=VERTEX_POINT('',#9281);
#2351=VERTEX_POINT('',#9289);
#2352=VERTEX_POINT('',#9290);
#2353=VERTEX_POINT('',#9292);
#2354=VERTEX_POINT('',#9299);
#2355=VERTEX_POINT('',#9307);
#2356=VERTEX_POINT('',#9308);
#2357=VERTEX_POINT('',#9310);
#2358=VERTEX_POINT('',#9317);
#2359=VERTEX_POINT('',#9325);
#2360=VERTEX_POINT('',#9332);
#2361=VERTEX_POINT('',#9363);
#2362=VERTEX_POINT('',#9365);
#2363=VERTEX_POINT('',#9369);
#2364=VERTEX_POINT('',#9371);
#2365=VERTEX_POINT('',#9375);
#2366=VERTEX_POINT('',#9377);
#2367=VERTEX_POINT('',#9381);
#2368=VERTEX_POINT('',#9383);
#2369=VERTEX_POINT('',#9387);
#2370=VERTEX_POINT('',#9389);
#2371=VERTEX_POINT('',#9393);
#2372=VERTEX_POINT('',#9395);
#2373=VERTEX_POINT('',#9399);
#2374=VERTEX_POINT('',#9401);
#2375=VERTEX_POINT('',#9409);
#2376=VERTEX_POINT('',#9411);
#2377=VERTEX_POINT('',#9415);
#2378=VERTEX_POINT('',#9417);
#2379=VERTEX_POINT('',#9424);
#2380=VERTEX_POINT('',#9426);
#2381=VERTEX_POINT('',#9430);
#2382=VERTEX_POINT('',#9431);
#2383=VERTEX_POINT('',#9433);
#2384=VERTEX_POINT('',#9435);
#2385=VERTEX_POINT('',#9437);
#2386=VERTEX_POINT('',#9439);
#2387=VERTEX_POINT('',#9443);
#2388=VERTEX_POINT('',#9444);
#2389=VERTEX_POINT('',#9449);
#2390=VERTEX_POINT('',#9453);
#2391=VERTEX_POINT('',#9457);
#2392=VERTEX_POINT('',#9461);
#2393=VERTEX_POINT('',#9470);
#2394=VERTEX_POINT('',#9471);
#2395=VERTEX_POINT('',#9473);
#2396=VERTEX_POINT('',#9485);
#2397=VERTEX_POINT('',#9501);
#2398=VERTEX_POINT('',#9502);
#2399=VERTEX_POINT('',#9539);
#2400=VERTEX_POINT('',#9540);
#2401=VERTEX_POINT('',#9577);
#2402=VERTEX_POINT('',#9578);
#2403=VERTEX_POINT('',#9580);
#2404=VERTEX_POINT('',#9588);
#2405=VERTEX_POINT('',#9600);
#2406=VERTEX_POINT('',#9601);
#2407=VERTEX_POINT('',#9603);
#2408=VERTEX_POINT('',#9605);
#2409=VERTEX_POINT('',#9620);
#2410=VERTEX_POINT('',#9621);
#2411=VERTEX_POINT('',#9623);
#2412=VERTEX_POINT('',#9638);
#2413=VERTEX_POINT('',#9640);
#2414=VERTEX_POINT('',#9653);
#2415=VERTEX_POINT('',#9654);
#2416=VERTEX_POINT('',#9721);
#2417=VERTEX_POINT('',#9722);
#2418=VERTEX_POINT('',#9797);
#2419=VERTEX_POINT('',#9798);
#2420=VERTEX_POINT('',#9892);
#2421=VERTEX_POINT('',#9893);
#2422=VERTEX_POINT('',#9897);
#2423=VERTEX_POINT('',#9901);
#2424=VERTEX_POINT('',#9905);
#2425=VERTEX_POINT('',#9909);
#2426=VERTEX_POINT('',#9912);
#2427=VERTEX_POINT('',#9916);
#2428=VERTEX_POINT('',#9924);
#2429=VERTEX_POINT('',#9953);
#2430=VERTEX_POINT('',#9990);
#2431=VERTEX_POINT('',#9991);
#2432=VERTEX_POINT('',#9993);
#2433=VERTEX_POINT('',#9995);
#2434=VERTEX_POINT('',#9997);
#2435=VERTEX_POINT('',#9999);
#2436=EDGE_CURVE('',#1917,#1917,#1476,.T.);
#2437=EDGE_CURVE('',#1917,#1918,#894,.T.);
#2438=EDGE_CURVE('',#1918,#1918,#1477,.T.);
#2439=EDGE_CURVE('',#1919,#1919,#1478,.T.);
#2440=EDGE_CURVE('',#1919,#1920,#895,.T.);
#2441=EDGE_CURVE('',#1920,#1920,#1479,.T.);
#2442=EDGE_CURVE('',#1921,#1921,#1480,.T.);
#2443=EDGE_CURVE('',#1921,#1922,#896,.T.);
#2444=EDGE_CURVE('',#1922,#1922,#1481,.T.);
#2445=EDGE_CURVE('',#1923,#1923,#1482,.T.);
#2446=EDGE_CURVE('',#1923,#1924,#897,.T.);
#2447=EDGE_CURVE('',#1924,#1924,#1483,.T.);
#2448=EDGE_CURVE('',#1925,#1925,#1484,.T.);
#2449=EDGE_CURVE('',#1925,#1926,#898,.T.);
#2450=EDGE_CURVE('',#1926,#1926,#1485,.T.);
#2451=EDGE_CURVE('',#1927,#1927,#1486,.T.);
#2452=EDGE_CURVE('',#1927,#1928,#899,.T.);
#2453=EDGE_CURVE('',#1928,#1928,#1487,.T.);
#2454=EDGE_CURVE('',#1929,#1929,#1488,.T.);
#2455=EDGE_CURVE('',#1929,#1930,#900,.T.);
#2456=EDGE_CURVE('',#1930,#1930,#1489,.T.);
#2457=EDGE_CURVE('',#1931,#1931,#1490,.T.);
#2458=EDGE_CURVE('',#1931,#1932,#901,.T.);
#2459=EDGE_CURVE('',#1932,#1932,#1491,.T.);
#2460=EDGE_CURVE('',#1933,#1933,#1492,.T.);
#2461=EDGE_CURVE('',#1933,#1934,#902,.T.);
#2462=EDGE_CURVE('',#1934,#1934,#1493,.T.);
#2463=EDGE_CURVE('',#1935,#1936,#903,.T.);
#2464=EDGE_CURVE('',#1935,#1937,#904,.T.);
#2465=EDGE_CURVE('',#1938,#1937,#905,.T.);
#2466=EDGE_CURVE('',#1938,#1936,#906,.T.);
#2467=EDGE_CURVE('',#1939,#1940,#907,.T.);
#2468=EDGE_CURVE('',#1941,#1939,#908,.T.);
#2469=EDGE_CURVE('',#1942,#1941,#909,.T.);
#2470=EDGE_CURVE('',#1940,#1942,#910,.T.);
#2471=EDGE_CURVE('',#1940,#1938,#911,.T.);
#2472=EDGE_CURVE('',#1942,#1943,#912,.T.);
#2473=EDGE_CURVE('',#1944,#1943,#913,.T.);
#2474=EDGE_CURVE('',#1944,#1936,#914,.T.);
#2475=EDGE_CURVE('',#1939,#1937,#915,.T.);
#2476=EDGE_CURVE('',#1945,#1935,#916,.T.);
#2477=EDGE_CURVE('',#1946,#1945,#917,.T.);
#2478=EDGE_CURVE('',#1941,#1946,#918,.T.);
#2479=EDGE_CURVE('',#1943,#1946,#919,.T.);
#2480=EDGE_CURVE('',#1945,#1944,#920,.T.);
#2481=EDGE_CURVE('',#1947,#1947,#1494,.T.);
#2482=EDGE_CURVE('',#1947,#1948,#921,.T.);
#2483=EDGE_CURVE('',#1948,#1948,#1495,.T.);
#2484=EDGE_CURVE('',#1949,#1950,#1496,.T.);
#2485=EDGE_CURVE('',#1950,#1951,#922,.T.);
#2486=EDGE_CURVE('',#1951,#1952,#1497,.T.);
#2487=EDGE_CURVE('',#1952,#1953,#923,.T.);
#2488=EDGE_CURVE('',#1953,#1953,#1498,.T.);
#2489=EDGE_CURVE('',#1952,#1954,#1499,.T.);
#2490=EDGE_CURVE('',#1949,#1954,#924,.T.);
#2491=EDGE_CURVE('',#1955,#1955,#1500,.T.);
#2492=EDGE_CURVE('',#1955,#1956,#925,.T.);
#2493=EDGE_CURVE('',#1957,#1956,#1501,.T.);
#2494=EDGE_CURVE('',#1958,#1957,#1502,.T.);
#2495=EDGE_CURVE('',#1956,#1958,#1503,.T.);
#2496=EDGE_CURVE('',#1959,#1959,#1504,.T.);
#2497=EDGE_CURVE('',#1959,#1960,#926,.T.);
#2498=EDGE_CURVE('',#1960,#1960,#1505,.T.);
#2499=EDGE_CURVE('',#1961,#1961,#1506,.T.);
#2500=EDGE_CURVE('',#1961,#1962,#927,.T.);
#2501=EDGE_CURVE('',#1962,#1962,#1507,.T.);
#2502=EDGE_CURVE('',#1954,#1958,#928,.T.);
#2503=EDGE_CURVE('',#1957,#1951,#929,.T.);
#2504=EDGE_CURVE('',#1958,#1963,#930,.T.);
#2505=EDGE_CURVE('',#1964,#1957,#931,.T.);
#2506=EDGE_CURVE('',#1963,#1964,#932,.T.);
#2507=EDGE_CURVE('',#1965,#1963,#933,.T.);
#2508=EDGE_CURVE('',#1949,#1965,#934,.T.);
#2509=EDGE_CURVE('',#1966,#1964,#935,.T.);
#2510=EDGE_CURVE('',#1965,#1966,#936,.T.);
#2511=EDGE_CURVE('',#1966,#1950,#937,.T.);
#2512=EDGE_CURVE('',#1967,#1968,#1508,.T.);
#2513=EDGE_CURVE('',#1967,#1969,#938,.T.);
#2514=EDGE_CURVE('',#1969,#1970,#1509,.T.);
#2515=EDGE_CURVE('',#1970,#1968,#939,.T.);
#2516=EDGE_CURVE('',#1971,#1972,#1510,.T.);
#2517=EDGE_CURVE('',#1973,#1971,#940,.T.);
#2518=EDGE_CURVE('',#1974,#1973,#1511,.T.);
#2519=EDGE_CURVE('',#1972,#1974,#941,.T.);
#2520=EDGE_CURVE('',#1975,#1974,#1512,.T.);
#2521=EDGE_CURVE('',#1976,#1975,#942,.T.);
#2522=EDGE_CURVE('',#1976,#1972,#1513,.T.);
#2523=EDGE_CURVE('',#1977,#1978,#1514,.T.);
#2524=EDGE_CURVE('',#1979,#1977,#943,.T.);
#2525=EDGE_CURVE('',#1980,#1979,#1515,.T.);
#2526=EDGE_CURVE('',#1978,#1980,#944,.T.);
#2527=EDGE_CURVE('',#1981,#1980,#1516,.T.);
#2528=EDGE_CURVE('',#1982,#1981,#945,.T.);
#2529=EDGE_CURVE('',#1982,#1978,#1517,.T.);
#2530=EDGE_CURVE('',#1983,#1984,#1518,.T.);
#2531=EDGE_CURVE('',#1985,#1983,#946,.T.);
#2532=EDGE_CURVE('',#1986,#1985,#1519,.T.);
#2533=EDGE_CURVE('',#1984,#1986,#947,.T.);
#2534=EDGE_CURVE('',#1985,#1987,#1520,.T.);
#2535=EDGE_CURVE('',#1983,#1988,#1521,.T.);
#2536=EDGE_CURVE('',#1987,#1988,#948,.T.);
#2537=EDGE_CURVE('',#1989,#1990,#1522,.T.);
#2538=EDGE_CURVE('',#1991,#1989,#949,.T.);
#2539=EDGE_CURVE('',#1992,#1991,#1523,.T.);
#2540=EDGE_CURVE('',#1990,#1992,#950,.T.);
#2541=EDGE_CURVE('',#1991,#1993,#1524,.T.);
#2542=EDGE_CURVE('',#1989,#1994,#1525,.T.);
#2543=EDGE_CURVE('',#1993,#1994,#951,.T.);
#2544=EDGE_CURVE('',#1995,#1996,#1526,.T.);
#2545=EDGE_CURVE('',#1997,#1995,#952,.T.);
#2546=EDGE_CURVE('',#1998,#1997,#1527,.T.);
#2547=EDGE_CURVE('',#1996,#1998,#953,.T.);
#2548=EDGE_CURVE('',#1999,#2000,#1528,.T.);
#2549=EDGE_CURVE('',#2001,#1999,#954,.T.);
#2550=EDGE_CURVE('',#2002,#2001,#1529,.T.);
#2551=EDGE_CURVE('',#2000,#2002,#955,.T.);
#2552=EDGE_CURVE('',#2003,#2004,#1530,.T.);
#2553=EDGE_CURVE('',#2005,#2003,#956,.T.);
#2554=EDGE_CURVE('',#2006,#2005,#1531,.T.);
#2555=EDGE_CURVE('',#2004,#2006,#957,.T.);
#2556=EDGE_CURVE('',#2007,#2008,#1532,.T.);
#2557=EDGE_CURVE('',#2009,#2007,#958,.T.);
#2558=EDGE_CURVE('',#2010,#2009,#1533,.T.);
#2559=EDGE_CURVE('',#2008,#2010,#959,.T.);
#2560=EDGE_CURVE('',#2011,#2012,#1534,.T.);
#2561=EDGE_CURVE('',#2013,#2011,#960,.T.);
#2562=EDGE_CURVE('',#2014,#2013,#1535,.T.);
#2563=EDGE_CURVE('',#2012,#2014,#961,.T.);
#2564=EDGE_CURVE('',#2015,#2016,#1536,.T.);
#2565=EDGE_CURVE('',#2017,#2015,#962,.T.);
#2566=EDGE_CURVE('',#2018,#2017,#1537,.T.);
#2567=EDGE_CURVE('',#2016,#2018,#963,.T.);
#2568=EDGE_CURVE('',#2019,#2020,#1538,.T.);
#2569=EDGE_CURVE('',#2021,#2019,#964,.T.);
#2570=EDGE_CURVE('',#2022,#2021,#1539,.T.);
#2571=EDGE_CURVE('',#2020,#2022,#965,.T.);
#2572=EDGE_CURVE('',#2023,#2024,#1540,.T.);
#2573=EDGE_CURVE('',#2025,#2023,#966,.T.);
#2574=EDGE_CURVE('',#2026,#2025,#1541,.T.);
#2575=EDGE_CURVE('',#2024,#2026,#967,.T.);
#2576=EDGE_CURVE('',#2027,#2028,#1542,.T.);
#2577=EDGE_CURVE('',#2029,#2027,#968,.T.);
#2578=EDGE_CURVE('',#2030,#2029,#1543,.T.);
#2579=EDGE_CURVE('',#2028,#2030,#969,.T.);
#2580=EDGE_CURVE('',#2031,#2032,#1544,.T.);
#2581=EDGE_CURVE('',#2033,#2031,#970,.T.);
#2582=EDGE_CURVE('',#2034,#2033,#1545,.T.);
#2583=EDGE_CURVE('',#2032,#2034,#971,.T.);
#2584=EDGE_CURVE('',#2035,#2036,#1546,.T.);
#2585=EDGE_CURVE('',#2035,#2037,#972,.T.);
#2586=EDGE_CURVE('',#2037,#2038,#1547,.T.);
#2587=EDGE_CURVE('',#2038,#2036,#973,.T.);
#2588=EDGE_CURVE('',#2039,#2040,#1548,.T.);
#2589=EDGE_CURVE('',#2039,#2041,#974,.T.);
#2590=EDGE_CURVE('',#2041,#2042,#1549,.T.);
#2591=EDGE_CURVE('',#2042,#2040,#975,.T.);
#2592=EDGE_CURVE('',#2043,#2044,#1550,.T.);
#2593=EDGE_CURVE('',#2044,#2045,#976,.T.);
#2594=EDGE_CURVE('',#2046,#2045,#1551,.T.);
#2595=EDGE_CURVE('',#2046,#2043,#977,.T.);
#2596=EDGE_CURVE('',#2047,#2048,#1552,.T.);
#2597=EDGE_CURVE('',#2047,#2049,#978,.T.);
#2598=EDGE_CURVE('',#2049,#2050,#1553,.T.);
#2599=EDGE_CURVE('',#2050,#2048,#979,.T.);
#2600=EDGE_CURVE('',#2051,#2052,#1554,.T.);
#2601=EDGE_CURVE('',#2051,#2053,#980,.T.);
#2602=EDGE_CURVE('',#2053,#2054,#1555,.T.);
#2603=EDGE_CURVE('',#2054,#2052,#981,.T.);
#2604=EDGE_CURVE('',#2055,#2056,#1556,.T.);
#2605=EDGE_CURVE('',#2056,#2057,#982,.T.);
#2606=EDGE_CURVE('',#2058,#2057,#1557,.T.);
#2607=EDGE_CURVE('',#2058,#2055,#983,.T.);
#2608=EDGE_CURVE('',#2059,#2060,#1558,.T.);
#2609=EDGE_CURVE('',#2060,#2061,#984,.T.);
#2610=EDGE_CURVE('',#2062,#2061,#1559,.T.);
#2611=EDGE_CURVE('',#2062,#2059,#985,.T.);
#2612=EDGE_CURVE('',#2063,#2064,#1560,.T.);
#2613=EDGE_CURVE('',#2064,#2065,#986,.T.);
#2614=EDGE_CURVE('',#2066,#2065,#1561,.T.);
#2615=EDGE_CURVE('',#2066,#2063,#987,.T.);
#2616=EDGE_CURVE('',#2067,#2068,#1562,.T.);
#2617=EDGE_CURVE('',#2067,#2069,#988,.T.);
#2618=EDGE_CURVE('',#2069,#2070,#1563,.T.);
#2619=EDGE_CURVE('',#2070,#2068,#989,.T.);
#2620=EDGE_CURVE('',#2071,#2072,#1564,.T.);
#2621=EDGE_CURVE('',#2071,#2073,#990,.T.);
#2622=EDGE_CURVE('',#2073,#2074,#1565,.T.);
#2623=EDGE_CURVE('',#2074,#2072,#991,.T.);
#2624=EDGE_CURVE('',#2075,#2076,#1566,.T.);
#2625=EDGE_CURVE('',#2076,#2077,#992,.T.);
#2626=EDGE_CURVE('',#2078,#2077,#1567,.T.);
#2627=EDGE_CURVE('',#2078,#2075,#993,.T.);
#2628=EDGE_CURVE('',#2079,#2080,#1568,.T.);
#2629=EDGE_CURVE('',#2080,#2081,#994,.T.);
#2630=EDGE_CURVE('',#2082,#2081,#1569,.T.);
#2631=EDGE_CURVE('',#2082,#2079,#995,.T.);
#2632=EDGE_CURVE('',#2083,#2084,#1570,.T.);
#2633=EDGE_CURVE('',#2084,#2085,#996,.T.);
#2634=EDGE_CURVE('',#2086,#2085,#1571,.T.);
#2635=EDGE_CURVE('',#2086,#2083,#997,.T.);
#2636=EDGE_CURVE('',#2087,#2088,#1572,.T.);
#2637=EDGE_CURVE('',#2088,#2089,#998,.T.);
#2638=EDGE_CURVE('',#2090,#2089,#1573,.T.);
#2639=EDGE_CURVE('',#2090,#2087,#999,.T.);
#2640=EDGE_CURVE('',#1975,#2091,#1574,.T.);
#2641=EDGE_CURVE('',#2091,#2092,#1000,.T.);
#2642=EDGE_CURVE('',#1976,#2092,#1575,.T.);
#2643=EDGE_CURVE('',#1981,#2093,#1576,.T.);
#2644=EDGE_CURVE('',#2093,#2094,#1001,.T.);
#2645=EDGE_CURVE('',#1982,#2094,#1577,.T.);
#2646=EDGE_CURVE('',#2095,#1994,#1578,.T.);
#2647=EDGE_CURVE('',#2095,#2096,#1002,.T.);
#2648=EDGE_CURVE('',#2096,#1993,#1579,.T.);
#2649=EDGE_CURVE('',#2097,#2098,#1580,.T.);
#2650=EDGE_CURVE('',#2097,#2099,#1003,.T.);
#2651=EDGE_CURVE('',#2099,#2100,#1581,.T.);
#2652=EDGE_CURVE('',#2100,#2098,#1004,.T.);
#2653=EDGE_CURVE('',#2101,#2102,#1582,.T.);
#2654=EDGE_CURVE('',#2101,#2103,#1005,.T.);
#2655=EDGE_CURVE('',#2103,#2104,#1583,.T.);
#2656=EDGE_CURVE('',#2104,#2102,#1006,.T.);
#2657=EDGE_CURVE('',#2105,#2106,#1584,.T.);
#2658=EDGE_CURVE('',#2106,#2107,#1007,.T.);
#2659=EDGE_CURVE('',#2108,#2107,#1585,.T.);
#2660=EDGE_CURVE('',#2108,#2105,#1008,.T.);
#2661=EDGE_CURVE('',#2109,#2110,#1586,.T.);
#2662=EDGE_CURVE('',#2109,#2111,#1009,.T.);
#2663=EDGE_CURVE('',#2111,#2112,#1587,.T.);
#2664=EDGE_CURVE('',#2112,#2110,#1010,.T.);
#2665=EDGE_CURVE('',#2113,#2114,#1588,.T.);
#2666=EDGE_CURVE('',#2113,#2115,#1011,.T.);
#2667=EDGE_CURVE('',#2115,#2116,#1589,.T.);
#2668=EDGE_CURVE('',#2116,#2114,#1012,.T.);
#2669=EDGE_CURVE('',#2117,#2118,#1590,.T.);
#2670=EDGE_CURVE('',#2117,#2119,#1013,.T.);
#2671=EDGE_CURVE('',#2119,#2120,#1591,.T.);
#2672=EDGE_CURVE('',#2120,#2118,#1014,.T.);
#2673=EDGE_CURVE('',#2121,#2122,#1592,.T.);
#2674=EDGE_CURVE('',#2121,#2123,#1015,.T.);
#2675=EDGE_CURVE('',#2123,#2124,#1593,.T.);
#2676=EDGE_CURVE('',#2124,#2122,#1016,.T.);
#2677=EDGE_CURVE('',#2125,#2126,#1594,.T.);
#2678=EDGE_CURVE('',#2125,#2127,#1017,.T.);
#2679=EDGE_CURVE('',#2127,#2128,#1595,.T.);
#2680=EDGE_CURVE('',#2128,#2126,#1018,.T.);
#2681=EDGE_CURVE('',#2129,#2130,#1596,.T.);
#2682=EDGE_CURVE('',#2130,#2131,#1019,.T.);
#2683=EDGE_CURVE('',#2132,#2131,#1597,.T.);
#2684=EDGE_CURVE('',#2132,#2129,#1020,.T.);
#2685=EDGE_CURVE('',#2133,#2134,#1598,.T.);
#2686=EDGE_CURVE('',#2134,#2135,#1021,.T.);
#2687=EDGE_CURVE('',#2136,#2135,#1599,.T.);
#2688=EDGE_CURVE('',#2136,#2133,#1022,.T.);
#2689=EDGE_CURVE('',#2137,#2138,#1600,.T.);
#2690=EDGE_CURVE('',#2138,#2139,#1023,.T.);
#2691=EDGE_CURVE('',#2140,#2139,#1601,.T.);
#2692=EDGE_CURVE('',#2140,#2137,#1024,.T.);
#2693=EDGE_CURVE('',#2141,#2142,#1602,.T.);
#2694=EDGE_CURVE('',#2141,#2143,#1025,.T.);
#2695=EDGE_CURVE('',#2143,#2144,#1603,.T.);
#2696=EDGE_CURVE('',#2144,#2142,#1026,.T.);
#2697=EDGE_CURVE('',#2041,#2145,#1604,.T.);
#2698=EDGE_CURVE('',#2145,#2146,#1605,.T.);
#2699=EDGE_CURVE('',#2146,#2147,#1606,.T.);
#2700=EDGE_CURVE('',#2147,#2148,#1607,.T.);
#2701=EDGE_CURVE('',#2148,#2044,#1608,.T.);
#2702=EDGE_CURVE('',#2043,#2149,#1609,.T.);
#2703=EDGE_CURVE('',#2149,#2150,#1610,.T.);
#2704=EDGE_CURVE('',#2150,#2151,#1611,.T.);
#2705=EDGE_CURVE('',#2151,#2152,#1612,.T.);
#2706=EDGE_CURVE('',#2152,#2056,#1613,.T.);
#2707=EDGE_CURVE('',#2055,#2153,#1614,.T.);
#2708=EDGE_CURVE('',#2153,#2154,#1615,.T.);
#2709=EDGE_CURVE('',#2154,#2155,#1616,.T.);
#2710=EDGE_CURVE('',#2155,#2156,#1617,.T.);
#2711=EDGE_CURVE('',#2156,#2060,#1618,.T.);
#2712=EDGE_CURVE('',#2059,#2157,#1619,.T.);
#2713=EDGE_CURVE('',#2157,#2158,#1620,.T.);
#2714=EDGE_CURVE('',#2158,#2159,#1621,.T.);
#2715=EDGE_CURVE('',#2159,#2160,#1622,.T.);
#2716=EDGE_CURVE('',#2160,#2038,#1623,.T.);
#2717=EDGE_CURVE('',#2037,#2161,#1624,.T.);
#2718=EDGE_CURVE('',#2161,#2162,#1625,.T.);
#2719=EDGE_CURVE('',#2162,#2163,#1626,.T.);
#2720=EDGE_CURVE('',#2163,#2164,#1627,.T.);
#2721=EDGE_CURVE('',#2164,#2064,#1628,.T.);
#2722=EDGE_CURVE('',#2063,#2165,#1629,.T.);
#2723=EDGE_CURVE('',#2165,#2166,#1630,.T.);
#2724=EDGE_CURVE('',#2166,#2167,#1631,.T.);
#2725=EDGE_CURVE('',#2167,#2168,#1632,.T.);
#2726=EDGE_CURVE('',#2168,#2076,#1633,.T.);
#2727=EDGE_CURVE('',#2075,#2169,#1634,.T.);
#2728=EDGE_CURVE('',#2169,#2170,#1635,.T.);
#2729=EDGE_CURVE('',#2170,#2171,#1636,.T.);
#2730=EDGE_CURVE('',#2171,#2172,#1637,.T.);
#2731=EDGE_CURVE('',#2172,#2080,#1638,.T.);
#2732=EDGE_CURVE('',#2079,#2173,#1639,.T.);
#2733=EDGE_CURVE('',#2173,#2174,#1640,.T.);
#2734=EDGE_CURVE('',#2174,#2175,#1641,.T.);
#2735=EDGE_CURVE('',#2175,#2176,#1642,.T.);
#2736=EDGE_CURVE('',#2176,#2074,#1643,.T.);
#2737=EDGE_CURVE('',#2073,#2177,#1644,.T.);
#2738=EDGE_CURVE('',#2177,#2178,#1645,.T.);
#2739=EDGE_CURVE('',#2178,#2179,#1646,.T.);
#2740=EDGE_CURVE('',#2179,#2180,#1647,.T.);
#2741=EDGE_CURVE('',#2180,#2070,#1648,.T.);
#2742=EDGE_CURVE('',#2069,#2181,#1649,.T.);
#2743=EDGE_CURVE('',#2181,#2182,#1650,.T.);
#2744=EDGE_CURVE('',#2182,#2183,#1651,.T.);
#2745=EDGE_CURVE('',#2183,#2184,#1652,.T.);
#2746=EDGE_CURVE('',#2184,#2084,#1653,.T.);
#2747=EDGE_CURVE('',#2083,#2185,#1654,.T.);
#2748=EDGE_CURVE('',#2185,#2186,#1655,.T.);
#2749=EDGE_CURVE('',#2186,#2187,#1656,.T.);
#2750=EDGE_CURVE('',#2187,#2188,#1657,.T.);
#2751=EDGE_CURVE('',#2188,#2088,#1658,.T.);
#2752=EDGE_CURVE('',#2087,#2189,#1659,.T.);
#2753=EDGE_CURVE('',#2189,#2190,#1660,.T.);
#2754=EDGE_CURVE('',#2190,#2191,#1661,.T.);
#2755=EDGE_CURVE('',#2191,#2192,#1662,.T.);
#2756=EDGE_CURVE('',#2192,#2091,#1663,.T.);
#2757=EDGE_CURVE('',#1973,#2193,#1664,.T.);
#2758=EDGE_CURVE('',#2193,#2194,#1665,.T.);
#2759=EDGE_CURVE('',#2194,#2093,#1666,.T.);
#2760=EDGE_CURVE('',#1979,#2195,#1667,.T.);
#2761=EDGE_CURVE('',#2195,#2196,#1668,.T.);
#2762=EDGE_CURVE('',#2196,#2130,#1669,.T.);
#2763=EDGE_CURVE('',#2129,#2026,#1670,.T.);
#2764=EDGE_CURVE('',#2025,#2197,#1671,.T.);
#2765=EDGE_CURVE('',#2197,#2198,#1672,.T.);
#2766=EDGE_CURVE('',#2198,#2128,#1673,.T.);
#2767=EDGE_CURVE('',#2127,#2022,#1674,.T.);
#2768=EDGE_CURVE('',#2021,#2199,#1675,.T.);
#2769=EDGE_CURVE('',#2199,#2200,#1676,.T.);
#2770=EDGE_CURVE('',#2200,#2134,#1677,.T.);
#2771=EDGE_CURVE('',#2133,#2030,#1678,.T.);
#2772=EDGE_CURVE('',#2029,#2201,#1679,.T.);
#2773=EDGE_CURVE('',#2201,#2202,#1680,.T.);
#2774=EDGE_CURVE('',#2202,#2138,#1681,.T.);
#2775=EDGE_CURVE('',#2137,#2034,#1682,.T.);
#2776=EDGE_CURVE('',#2033,#2203,#1683,.T.);
#2777=EDGE_CURVE('',#2203,#2204,#1684,.T.);
#2778=EDGE_CURVE('',#2204,#2124,#1685,.T.);
#2779=EDGE_CURVE('',#2123,#2018,#1686,.T.);
#2780=EDGE_CURVE('',#2017,#2205,#1687,.T.);
#2781=EDGE_CURVE('',#2205,#2206,#1688,.T.);
#2782=EDGE_CURVE('',#2206,#2120,#1689,.T.);
#2783=EDGE_CURVE('',#2119,#2207,#1690,.T.);
#2784=EDGE_CURVE('',#2207,#2208,#1691,.T.);
#2785=EDGE_CURVE('',#2208,#2014,#1692,.T.);
#2786=EDGE_CURVE('',#2013,#2116,#1693,.T.);
#2787=EDGE_CURVE('',#2115,#2209,#1694,.T.);
#2788=EDGE_CURVE('',#2209,#2210,#1695,.T.);
#2789=EDGE_CURVE('',#2210,#2010,#1696,.T.);
#2790=EDGE_CURVE('',#2009,#2112,#1697,.T.);
#2791=EDGE_CURVE('',#2111,#2211,#1698,.T.);
#2792=EDGE_CURVE('',#2211,#2212,#1699,.T.);
#2793=EDGE_CURVE('',#2212,#2006,#1700,.T.);
#2794=EDGE_CURVE('',#2005,#2104,#1701,.T.);
#2795=EDGE_CURVE('',#2103,#2213,#1702,.T.);
#2796=EDGE_CURVE('',#2213,#2214,#1703,.T.);
#2797=EDGE_CURVE('',#2214,#1998,#1704,.T.);
#2798=EDGE_CURVE('',#1997,#2106,#1705,.T.);
#2799=EDGE_CURVE('',#2105,#2215,#1706,.T.);
#2800=EDGE_CURVE('',#2215,#2216,#1707,.T.);
#2801=EDGE_CURVE('',#2216,#2002,#1708,.T.);
#2802=EDGE_CURVE('',#2001,#2100,#1709,.T.);
#2803=EDGE_CURVE('',#2099,#2217,#1710,.T.);
#2804=EDGE_CURVE('',#2217,#2218,#1711,.T.);
#2805=EDGE_CURVE('',#2218,#1992,#1712,.T.);
#2806=EDGE_CURVE('',#2096,#2219,#1713,.T.);
#2807=EDGE_CURVE('',#2219,#2220,#1714,.T.);
#2808=EDGE_CURVE('',#2220,#1986,#1715,.T.);
#2809=EDGE_CURVE('',#2221,#1987,#1716,.T.);
#2810=EDGE_CURVE('',#2221,#2222,#1717,.T.);
#2811=EDGE_CURVE('',#2222,#2223,#1718,.T.);
#2812=EDGE_CURVE('',#2223,#2224,#1719,.T.);
#2813=EDGE_CURVE('',#2224,#2225,#1720,.T.);
#2814=EDGE_CURVE('',#2225,#2144,#1721,.T.);
#2815=EDGE_CURVE('',#2143,#2226,#1722,.T.);
#2816=EDGE_CURVE('',#2226,#2227,#1723,.T.);
#2817=EDGE_CURVE('',#2227,#2228,#1724,.T.);
#2818=EDGE_CURVE('',#2228,#2229,#1725,.T.);
#2819=EDGE_CURVE('',#2229,#2054,#1726,.T.);
#2820=EDGE_CURVE('',#2053,#2230,#1727,.T.);
#2821=EDGE_CURVE('',#2230,#2231,#1728,.T.);
#2822=EDGE_CURVE('',#2231,#2232,#1729,.T.);
#2823=EDGE_CURVE('',#2232,#2233,#1730,.T.);
#2824=EDGE_CURVE('',#2233,#2050,#1731,.T.);
#2825=EDGE_CURVE('',#2049,#2234,#1732,.T.);
#2826=EDGE_CURVE('',#2234,#2235,#1733,.T.);
#2827=EDGE_CURVE('',#2235,#2236,#1734,.T.);
#2828=EDGE_CURVE('',#2236,#2237,#1735,.T.);
#2829=EDGE_CURVE('',#2237,#2042,#1736,.T.);
#2830=EDGE_CURVE('',#2238,#2239,#1027,.T.);
#2831=EDGE_CURVE('',#2239,#1967,#1028,.T.);
#2832=EDGE_CURVE('',#1968,#2238,#1029,.T.);
#2833=EDGE_CURVE('',#2039,#2240,#1737,.T.);
#2834=EDGE_CURVE('',#2241,#2040,#1738,.T.);
#2835=EDGE_CURVE('',#2241,#2242,#1739,.T.);
#2836=EDGE_CURVE('',#2243,#2242,#1740,.T.);
#2837=EDGE_CURVE('',#2243,#2244,#1741,.T.);
#2838=EDGE_CURVE('',#2047,#2244,#1742,.T.);
#2839=EDGE_CURVE('',#2245,#2048,#1743,.T.);
#2840=EDGE_CURVE('',#2245,#2246,#1744,.T.);
#2841=EDGE_CURVE('',#2247,#2246,#1745,.T.);
#2842=EDGE_CURVE('',#2247,#2248,#1746,.T.);
#2843=EDGE_CURVE('',#2051,#2248,#1747,.T.);
#2844=EDGE_CURVE('',#2249,#2052,#1748,.T.);
#2845=EDGE_CURVE('',#2249,#2250,#1749,.T.);
#2846=EDGE_CURVE('',#2251,#2250,#1750,.T.);
#2847=EDGE_CURVE('',#2251,#2252,#1751,.T.);
#2848=EDGE_CURVE('',#2141,#2252,#1752,.T.);
#2849=EDGE_CURVE('',#2253,#2142,#1753,.T.);
#2850=EDGE_CURVE('',#2253,#2254,#1754,.T.);
#2851=EDGE_CURVE('',#2255,#2254,#1755,.T.);
#2852=EDGE_CURVE('',#2255,#2256,#1756,.T.);
#2853=EDGE_CURVE('',#2257,#2256,#1757,.T.);
#2854=EDGE_CURVE('',#2257,#1988,#1758,.T.);
#2855=EDGE_CURVE('',#2258,#1984,#1759,.T.);
#2856=EDGE_CURVE('',#2258,#2259,#1760,.T.);
#2857=EDGE_CURVE('',#2095,#2259,#1761,.T.);
#2858=EDGE_CURVE('',#2260,#1990,#1762,.T.);
#2859=EDGE_CURVE('',#2260,#2261,#1763,.T.);
#2860=EDGE_CURVE('',#2097,#2261,#1764,.T.);
#2861=EDGE_CURVE('',#1999,#2098,#1765,.T.);
#2862=EDGE_CURVE('',#2262,#2000,#1766,.T.);
#2863=EDGE_CURVE('',#2262,#2263,#1767,.T.);
#2864=EDGE_CURVE('',#2108,#2263,#1768,.T.);
#2865=EDGE_CURVE('',#1995,#2107,#1769,.T.);
#2866=EDGE_CURVE('',#2264,#1996,#1770,.T.);
#2867=EDGE_CURVE('',#2264,#2265,#1771,.T.);
#2868=EDGE_CURVE('',#2101,#2265,#1772,.T.);
#2869=EDGE_CURVE('',#2003,#2102,#1773,.T.);
#2870=EDGE_CURVE('',#2266,#2004,#1774,.T.);
#2871=EDGE_CURVE('',#2266,#2267,#1775,.T.);
#2872=EDGE_CURVE('',#2109,#2267,#1776,.T.);
#2873=EDGE_CURVE('',#2007,#2110,#1777,.T.);
#2874=EDGE_CURVE('',#2268,#2008,#1778,.T.);
#2875=EDGE_CURVE('',#2268,#2269,#1779,.T.);
#2876=EDGE_CURVE('',#2113,#2269,#1780,.T.);
#2877=EDGE_CURVE('',#2011,#2114,#1781,.T.);
#2878=EDGE_CURVE('',#2270,#2012,#1782,.T.);
#2879=EDGE_CURVE('',#2270,#2271,#1783,.T.);
#2880=EDGE_CURVE('',#2117,#2271,#1784,.T.);
#2881=EDGE_CURVE('',#2272,#2118,#1785,.T.);
#2882=EDGE_CURVE('',#2272,#2273,#1786,.T.);
#2883=EDGE_CURVE('',#2015,#2273,#1787,.T.);
#2884=EDGE_CURVE('',#2121,#2016,#1788,.T.);
#2885=EDGE_CURVE('',#2274,#2122,#1789,.T.);
#2886=EDGE_CURVE('',#2274,#2275,#1790,.T.);
#2887=EDGE_CURVE('',#2031,#2275,#1791,.T.);
#2888=EDGE_CURVE('',#2140,#2032,#1792,.T.);
#2889=EDGE_CURVE('',#2276,#2139,#1793,.T.);
#2890=EDGE_CURVE('',#2276,#2277,#1794,.T.);
#2891=EDGE_CURVE('',#2027,#2277,#1795,.T.);
#2892=EDGE_CURVE('',#2136,#2028,#1796,.T.);
#2893=EDGE_CURVE('',#2278,#2135,#1797,.T.);
#2894=EDGE_CURVE('',#2278,#2279,#1798,.T.);
#2895=EDGE_CURVE('',#2019,#2279,#1799,.T.);
#2896=EDGE_CURVE('',#2125,#2020,#1800,.T.);
#2897=EDGE_CURVE('',#2280,#2126,#1801,.T.);
#2898=EDGE_CURVE('',#2280,#2281,#1802,.T.);
#2899=EDGE_CURVE('',#2023,#2281,#1803,.T.);
#2900=EDGE_CURVE('',#2132,#2024,#1804,.T.);
#2901=EDGE_CURVE('',#2282,#2131,#1805,.T.);
#2902=EDGE_CURVE('',#2282,#2283,#1806,.T.);
#2903=EDGE_CURVE('',#1977,#2283,#1807,.T.);
#2904=EDGE_CURVE('',#2284,#2094,#1808,.T.);
#2905=EDGE_CURVE('',#2284,#2285,#1809,.T.);
#2906=EDGE_CURVE('',#1971,#2285,#1810,.T.);
#2907=EDGE_CURVE('',#2286,#2092,#1811,.T.);
#2908=EDGE_CURVE('',#2286,#2287,#1812,.T.);
#2909=EDGE_CURVE('',#2288,#2287,#1813,.T.);
#2910=EDGE_CURVE('',#2288,#2289,#1814,.T.);
#2911=EDGE_CURVE('',#2090,#2289,#1815,.T.);
#2912=EDGE_CURVE('',#2290,#2089,#1816,.T.);
#2913=EDGE_CURVE('',#2290,#2291,#1817,.T.);
#2914=EDGE_CURVE('',#2292,#2291,#1818,.T.);
#2915=EDGE_CURVE('',#2292,#2293,#1819,.T.);
#2916=EDGE_CURVE('',#2086,#2293,#1820,.T.);
#2917=EDGE_CURVE('',#2294,#2085,#1821,.T.);
#2918=EDGE_CURVE('',#2294,#2295,#1822,.T.);
#2919=EDGE_CURVE('',#2296,#2295,#1823,.T.);
#2920=EDGE_CURVE('',#2296,#2297,#1824,.T.);
#2921=EDGE_CURVE('',#2067,#2297,#1825,.T.);
#2922=EDGE_CURVE('',#2298,#2068,#1826,.T.);
#2923=EDGE_CURVE('',#2298,#2299,#1827,.T.);
#2924=EDGE_CURVE('',#2300,#2299,#1828,.T.);
#2925=EDGE_CURVE('',#2300,#2301,#1829,.T.);
#2926=EDGE_CURVE('',#2071,#2301,#1830,.T.);
#2927=EDGE_CURVE('',#2302,#2072,#1831,.T.);
#2928=EDGE_CURVE('',#2302,#2303,#1832,.T.);
#2929=EDGE_CURVE('',#2304,#2303,#1833,.T.);
#2930=EDGE_CURVE('',#2304,#2305,#1834,.T.);
#2931=EDGE_CURVE('',#2082,#2305,#1835,.T.);
#2932=EDGE_CURVE('',#2306,#2081,#1836,.T.);
#2933=EDGE_CURVE('',#2306,#2307,#1837,.T.);
#2934=EDGE_CURVE('',#2308,#2307,#1838,.T.);
#2935=EDGE_CURVE('',#2308,#2309,#1839,.T.);
#2936=EDGE_CURVE('',#2078,#2309,#1840,.T.);
#2937=EDGE_CURVE('',#2310,#2077,#1841,.T.);
#2938=EDGE_CURVE('',#2310,#2311,#1842,.T.);
#2939=EDGE_CURVE('',#2312,#2311,#1843,.T.);
#2940=EDGE_CURVE('',#2312,#2313,#1844,.T.);
#2941=EDGE_CURVE('',#2066,#2313,#1845,.T.);
#2942=EDGE_CURVE('',#2314,#2065,#1846,.T.);
#2943=EDGE_CURVE('',#2314,#2315,#1847,.T.);
#2944=EDGE_CURVE('',#2316,#2315,#1848,.T.);
#2945=EDGE_CURVE('',#2316,#2317,#1849,.T.);
#2946=EDGE_CURVE('',#2035,#2317,#1850,.T.);
#2947=EDGE_CURVE('',#2318,#2036,#1851,.T.);
#2948=EDGE_CURVE('',#2318,#2319,#1852,.T.);
#2949=EDGE_CURVE('',#2320,#2319,#1853,.T.);
#2950=EDGE_CURVE('',#2320,#2321,#1854,.T.);
#2951=EDGE_CURVE('',#2062,#2321,#1855,.T.);
#2952=EDGE_CURVE('',#2322,#2061,#1856,.T.);
#2953=EDGE_CURVE('',#2322,#2323,#1857,.T.);
#2954=EDGE_CURVE('',#2324,#2323,#1858,.T.);
#2955=EDGE_CURVE('',#2324,#2325,#1859,.T.);
#2956=EDGE_CURVE('',#2058,#2325,#1860,.T.);
#2957=EDGE_CURVE('',#2326,#2057,#1861,.T.);
#2958=EDGE_CURVE('',#2326,#2327,#1862,.T.);
#2959=EDGE_CURVE('',#2328,#2327,#1863,.T.);
#2960=EDGE_CURVE('',#2328,#2329,#1864,.T.);
#2961=EDGE_CURVE('',#2046,#2329,#1865,.T.);
#2962=EDGE_CURVE('',#2330,#2045,#1866,.T.);
#2963=EDGE_CURVE('',#2330,#2331,#1867,.T.);
#2964=EDGE_CURVE('',#2332,#2331,#1868,.T.);
#2965=EDGE_CURVE('',#2332,#2240,#1869,.T.);
#2966=EDGE_CURVE('',#2333,#1969,#1030,.T.);
#2967=EDGE_CURVE('',#2334,#2333,#1031,.T.);
#2968=EDGE_CURVE('',#1970,#2334,#1032,.T.);
#2969=EDGE_CURVE('',#2257,#2221,#1033,.T.);
#2970=EDGE_CURVE('',#2225,#2253,#1034,.T.);
#2971=EDGE_CURVE('',#2256,#2222,#1035,.T.);
#2972=EDGE_CURVE('',#2254,#2224,#1036,.T.);
#2973=EDGE_CURVE('',#2223,#2255,#1037,.T.);
#2974=EDGE_CURVE('',#2252,#2226,#1038,.T.);
#2975=EDGE_CURVE('',#2229,#2249,#1039,.T.);
#2976=EDGE_CURVE('',#2250,#2228,#1040,.T.);
#2977=EDGE_CURVE('',#2227,#2251,#1041,.T.);
#2978=EDGE_CURVE('',#2204,#2274,#1042,.T.);
#2979=EDGE_CURVE('',#2275,#2203,#1043,.T.);
#2980=EDGE_CURVE('',#2202,#2276,#1044,.T.);
#2981=EDGE_CURVE('',#2277,#2201,#1045,.T.);
#2982=EDGE_CURVE('',#2198,#2280,#1046,.T.);
#2983=EDGE_CURVE('',#2281,#2197,#1047,.T.);
#2984=EDGE_CURVE('',#2200,#2278,#1048,.T.);
#2985=EDGE_CURVE('',#2279,#2199,#1049,.T.);
#2986=EDGE_CURVE('',#2206,#2272,#1050,.T.);
#2987=EDGE_CURVE('',#2273,#2205,#1051,.T.);
#2988=EDGE_CURVE('',#2271,#2207,#1052,.T.);
#2989=EDGE_CURVE('',#2208,#2270,#1053,.T.);
#2990=EDGE_CURVE('',#2269,#2209,#1054,.T.);
#2991=EDGE_CURVE('',#2210,#2268,#1055,.T.);
#2992=EDGE_CURVE('',#2267,#2211,#1056,.T.);
#2993=EDGE_CURVE('',#2212,#2266,#1057,.T.);
#2994=EDGE_CURVE('',#2263,#2215,#1058,.T.);
#2995=EDGE_CURVE('',#2216,#2262,#1059,.T.);
#2996=EDGE_CURVE('',#2265,#2213,#1060,.T.);
#2997=EDGE_CURVE('',#2214,#2264,#1061,.T.);
#2998=EDGE_CURVE('',#2261,#2217,#1062,.T.);
#2999=EDGE_CURVE('',#2218,#2260,#1063,.T.);
#3000=EDGE_CURVE('',#2259,#2219,#1064,.T.);
#3001=EDGE_CURVE('',#2220,#2258,#1065,.T.);
#3002=EDGE_CURVE('',#2196,#2282,#1066,.T.);
#3003=EDGE_CURVE('',#2283,#2195,#1067,.T.);
#3004=EDGE_CURVE('',#2194,#2284,#1068,.T.);
#3005=EDGE_CURVE('',#2285,#2193,#1069,.T.);
#3006=EDGE_CURVE('',#2289,#2189,#1070,.T.);
#3007=EDGE_CURVE('',#2192,#2286,#1071,.T.);
#3008=EDGE_CURVE('',#2287,#2191,#1072,.T.);
#3009=EDGE_CURVE('',#2190,#2288,#1073,.T.);
#3010=EDGE_CURVE('',#2293,#2185,#1074,.T.);
#3011=EDGE_CURVE('',#2188,#2290,#1075,.T.);
#3012=EDGE_CURVE('',#2291,#2187,#1076,.T.);
#3013=EDGE_CURVE('',#2186,#2292,#1077,.T.);
#3014=EDGE_CURVE('',#2305,#2173,#1078,.T.);
#3015=EDGE_CURVE('',#2176,#2302,#1079,.T.);
#3016=EDGE_CURVE('',#2303,#2175,#1080,.T.);
#3017=EDGE_CURVE('',#2174,#2304,#1081,.T.);
#3018=EDGE_CURVE('',#2309,#2169,#1082,.T.);
#3019=EDGE_CURVE('',#2172,#2306,#1083,.T.);
#3020=EDGE_CURVE('',#2307,#2171,#1084,.T.);
#3021=EDGE_CURVE('',#2170,#2308,#1085,.T.);
#3022=EDGE_CURVE('',#2301,#2177,#1086,.T.);
#3023=EDGE_CURVE('',#2180,#2298,#1087,.T.);
#3024=EDGE_CURVE('',#2299,#2179,#1088,.T.);
#3025=EDGE_CURVE('',#2178,#2300,#1089,.T.);
#3026=EDGE_CURVE('',#2297,#2181,#1090,.T.);
#3027=EDGE_CURVE('',#2184,#2294,#1091,.T.);
#3028=EDGE_CURVE('',#2295,#2183,#1092,.T.);
#3029=EDGE_CURVE('',#2182,#2296,#1093,.T.);
#3030=EDGE_CURVE('',#2313,#2165,#1094,.T.);
#3031=EDGE_CURVE('',#2168,#2310,#1095,.T.);
#3032=EDGE_CURVE('',#2311,#2167,#1096,.T.);
#3033=EDGE_CURVE('',#2166,#2312,#1097,.T.);
#3034=EDGE_CURVE('',#2317,#2161,#1098,.T.);
#3035=EDGE_CURVE('',#2164,#2314,#1099,.T.);
#3036=EDGE_CURVE('',#2315,#2163,#1100,.T.);
#3037=EDGE_CURVE('',#2162,#2316,#1101,.T.);
#3038=EDGE_CURVE('',#2321,#2157,#1102,.T.);
#3039=EDGE_CURVE('',#2160,#2318,#1103,.T.);
#3040=EDGE_CURVE('',#2319,#2159,#1104,.T.);
#3041=EDGE_CURVE('',#2158,#2320,#1105,.T.);
#3042=EDGE_CURVE('',#2325,#2153,#1106,.T.);
#3043=EDGE_CURVE('',#2156,#2322,#1107,.T.);
#3044=EDGE_CURVE('',#2323,#2155,#1108,.T.);
#3045=EDGE_CURVE('',#2154,#2324,#1109,.T.);
#3046=EDGE_CURVE('',#2248,#2230,#1110,.T.);
#3047=EDGE_CURVE('',#2233,#2245,#1111,.T.);
#3048=EDGE_CURVE('',#2246,#2232,#1112,.T.);
#3049=EDGE_CURVE('',#2231,#2247,#1113,.T.);
#3050=EDGE_CURVE('',#2244,#2234,#1114,.T.);
#3051=EDGE_CURVE('',#2237,#2241,#1115,.T.);
#3052=EDGE_CURVE('',#2242,#2236,#1116,.T.);
#3053=EDGE_CURVE('',#2235,#2243,#1117,.T.);
#3054=EDGE_CURVE('',#2329,#2149,#1118,.T.);
#3055=EDGE_CURVE('',#2152,#2326,#1119,.T.);
#3056=EDGE_CURVE('',#2327,#2151,#1120,.T.);
#3057=EDGE_CURVE('',#2150,#2328,#1121,.T.);
#3058=EDGE_CURVE('',#2240,#2145,#1122,.T.);
#3059=EDGE_CURVE('',#2148,#2330,#1123,.T.);
#3060=EDGE_CURVE('',#2331,#2147,#1124,.T.);
#3061=EDGE_CURVE('',#2146,#2332,#1125,.T.);
#3062=EDGE_CURVE('',#2238,#2334,#1126,.T.);
#3063=EDGE_CURVE('',#2239,#2333,#1127,.T.);
#3064=EDGE_CURVE('',#2335,#2335,#1870,.T.);
#3065=EDGE_CURVE('',#2335,#2336,#1128,.T.);
#3066=EDGE_CURVE('',#2336,#2336,#1871,.T.);
#3067=EDGE_CURVE('',#2337,#2338,#1872,.T.);
#3068=EDGE_CURVE('',#2339,#2338,#90,.T.);
#3069=EDGE_CURVE('',#2337,#2339,#91,.T.);
#3070=EDGE_CURVE('',#2340,#2341,#1873,.T.);
#3071=EDGE_CURVE('',#2341,#2342,#92,.T.);
#3072=EDGE_CURVE('',#2342,#2340,#93,.T.);
#3073=EDGE_CURVE('',#2339,#2342,#1129,.T.);
#3074=EDGE_CURVE('',#2338,#2343,#94,.T.);
#3075=EDGE_CURVE('',#2343,#2344,#1130,.T.);
#3076=EDGE_CURVE('',#2340,#2344,#95,.T.);
#3077=EDGE_CURVE('',#2345,#2346,#1131,.T.);
#3078=EDGE_CURVE('',#2345,#2337,#96,.T.);
#3079=EDGE_CURVE('',#2346,#2341,#97,.T.);
#3080=EDGE_CURVE('',#2347,#2348,#1132,.T.);
#3081=EDGE_CURVE('',#2347,#2349,#98,.T.);
#3082=EDGE_CURVE('',#2349,#2345,#99,.T.);
#3083=EDGE_CURVE('',#2350,#2346,#100,.T.);
#3084=EDGE_CURVE('',#2348,#2350,#101,.T.);
#3085=EDGE_CURVE('',#2351,#2352,#1133,.T.);
#3086=EDGE_CURVE('',#2351,#2353,#102,.T.);
#3087=EDGE_CURVE('',#2353,#2347,#103,.T.);
#3088=EDGE_CURVE('',#2354,#2348,#104,.T.);
#3089=EDGE_CURVE('',#2352,#2354,#105,.T.);
#3090=EDGE_CURVE('',#2355,#2356,#1134,.T.);
#3091=EDGE_CURVE('',#2355,#2357,#106,.T.);
#3092=EDGE_CURVE('',#2357,#2351,#107,.T.);
#3093=EDGE_CURVE('',#2358,#2352,#108,.T.);
#3094=EDGE_CURVE('',#2356,#2358,#109,.T.);
#3095=EDGE_CURVE('',#2343,#2359,#110,.T.);
#3096=EDGE_CURVE('',#2359,#2355,#111,.T.);
#3097=EDGE_CURVE('',#2360,#2356,#112,.T.);
#3098=EDGE_CURVE('',#2344,#2360,#113,.T.);
#3099=EDGE_CURVE('',#2354,#2358,#1874,.T.);
#3100=EDGE_CURVE('',#2350,#2354,#1875,.T.);
#3101=EDGE_CURVE('',#2341,#2350,#1876,.T.);
#3102=EDGE_CURVE('',#2340,#2360,#1877,.T.);
#3103=EDGE_CURVE('',#2358,#2360,#1878,.T.);
#3104=EDGE_CURVE('',#2357,#2353,#1879,.T.);
#3105=EDGE_CURVE('',#2359,#2357,#1880,.T.);
#3106=EDGE_CURVE('',#2338,#2359,#1881,.T.);
#3107=EDGE_CURVE('',#2349,#2337,#1882,.T.);
#3108=EDGE_CURVE('',#2353,#2349,#1883,.T.);
#3109=EDGE_CURVE('',#2361,#2361,#1884,.T.);
#3110=EDGE_CURVE('',#2361,#2362,#1135,.T.);
#3111=EDGE_CURVE('',#2362,#2362,#1885,.T.);
#3112=EDGE_CURVE('',#2363,#2363,#1886,.T.);
#3113=EDGE_CURVE('',#2363,#2364,#1136,.T.);
#3114=EDGE_CURVE('',#2364,#2364,#1887,.T.);
#3115=EDGE_CURVE('',#2365,#2365,#1888,.T.);
#3116=EDGE_CURVE('',#2365,#2366,#1137,.T.);
#3117=EDGE_CURVE('',#2366,#2366,#1889,.T.);
#3118=EDGE_CURVE('',#2367,#2367,#1890,.T.);
#3119=EDGE_CURVE('',#2367,#2368,#1138,.T.);
#3120=EDGE_CURVE('',#2368,#2368,#1891,.T.);
#3121=EDGE_CURVE('',#2369,#2369,#1892,.T.);
#3122=EDGE_CURVE('',#2369,#2370,#1139,.T.);
#3123=EDGE_CURVE('',#2370,#2370,#1893,.T.);
#3124=EDGE_CURVE('',#2371,#2371,#1894,.T.);
#3125=EDGE_CURVE('',#2371,#2372,#1140,.T.);
#3126=EDGE_CURVE('',#2372,#2372,#1895,.T.);
#3127=EDGE_CURVE('',#2373,#2373,#1896,.T.);
#3128=EDGE_CURVE('',#2373,#2374,#1141,.T.);
#3129=EDGE_CURVE('',#2374,#2374,#1897,.T.);
#3130=EDGE_CURVE('',#2375,#2375,#1898,.T.);
#3131=EDGE_CURVE('',#2375,#2376,#1142,.T.);
#3132=EDGE_CURVE('',#2376,#2376,#1899,.T.);
#3133=EDGE_CURVE('',#2377,#2377,#1900,.T.);
#3134=EDGE_CURVE('',#2377,#2378,#1143,.T.);
#3135=EDGE_CURVE('',#2378,#2378,#1901,.T.);
#3136=EDGE_CURVE('',#2379,#2379,#1902,.T.);
#3137=EDGE_CURVE('',#2379,#2380,#1144,.T.);
#3138=EDGE_CURVE('',#2380,#2380,#1903,.T.);
#3139=EDGE_CURVE('',#2381,#2382,#1145,.T.);
#3140=EDGE_CURVE('',#2382,#2383,#1146,.T.);
#3141=EDGE_CURVE('',#2383,#2384,#1147,.T.);
#3142=EDGE_CURVE('',#2384,#2385,#1148,.T.);
#3143=EDGE_CURVE('',#2385,#2386,#1149,.T.);
#3144=EDGE_CURVE('',#2386,#2381,#1150,.T.);
#3145=EDGE_CURVE('',#2387,#2388,#1151,.T.);
#3146=EDGE_CURVE('',#2382,#2388,#1152,.T.);
#3147=EDGE_CURVE('',#2381,#2387,#1153,.T.);
#3148=EDGE_CURVE('',#2388,#2389,#1154,.T.);
#3149=EDGE_CURVE('',#2383,#2389,#1155,.T.);
#3150=EDGE_CURVE('',#2389,#2390,#1156,.T.);
#3151=EDGE_CURVE('',#2384,#2390,#1157,.T.);
#3152=EDGE_CURVE('',#2390,#2391,#1158,.T.);
#3153=EDGE_CURVE('',#2385,#2391,#1159,.T.);
#3154=EDGE_CURVE('',#2391,#2392,#1160,.T.);
#3155=EDGE_CURVE('',#2386,#2392,#1161,.T.);
#3156=EDGE_CURVE('',#2392,#2387,#1162,.T.);
#3157=EDGE_CURVE('',#2393,#2394,#1163,.T.);
#3158=EDGE_CURVE('',#2394,#2395,#114,.T.);
#3159=EDGE_CURVE('',#2395,#2396,#1904,.T.);
#3160=EDGE_CURVE('',#2393,#2396,#115,.T.);
#3161=EDGE_CURVE('',#2397,#2398,#1164,.T.);
#3162=EDGE_CURVE('',#2398,#2394,#116,.T.);
#3163=EDGE_CURVE('',#2397,#2393,#117,.T.);
#3164=EDGE_CURVE('',#2399,#2400,#1165,.T.);
#3165=EDGE_CURVE('',#2400,#2398,#118,.T.);
#3166=EDGE_CURVE('',#2399,#2397,#119,.T.);
#3167=EDGE_CURVE('',#2401,#2402,#1166,.T.);
#3168=EDGE_CURVE('',#2403,#2401,#120,.T.);
#3169=EDGE_CURVE('',#2403,#2404,#1905,.T.);
#3170=EDGE_CURVE('',#2404,#2402,#121,.T.);
#3171=EDGE_CURVE('',#2405,#2406,#1167,.T.);
#3172=EDGE_CURVE('',#2407,#2405,#1906,.T.);
#3173=EDGE_CURVE('',#2407,#2408,#77,.T.);
#3174=EDGE_CURVE('',#2408,#2406,#1907,.T.);
#3175=EDGE_CURVE('',#2409,#2410,#1168,.T.);
#3176=EDGE_CURVE('',#2409,#2411,#78,.T.);
#3177=EDGE_CURVE('',#2411,#2412,#1908,.T.);
#3178=EDGE_CURVE('',#2412,#2413,#79,.T.);
#3179=EDGE_CURVE('',#2410,#2413,#1909,.T.);
#3180=EDGE_CURVE('',#2414,#2415,#1169,.T.);
#3181=EDGE_CURVE('',#2407,#2415,#80,.F.);
#3182=EDGE_CURVE('',#2405,#2414,#81,.T.);
#3183=EDGE_CURVE('',#2416,#2417,#1170,.T.);
#3184=EDGE_CURVE('',#2415,#2417,#82,.F.);
#3185=EDGE_CURVE('',#2414,#2416,#83,.T.);
#3186=EDGE_CURVE('',#2418,#2419,#1171,.T.);
#3187=EDGE_CURVE('',#2418,#2412,#84,.T.);
#3188=EDGE_CURVE('',#2419,#2411,#85,.F.);
#3189=EDGE_CURVE('',#2417,#2419,#86,.F.);
#3190=EDGE_CURVE('',#2416,#2418,#87,.T.);
#3191=EDGE_CURVE('',#2420,#2421,#122,.T.);
#3192=EDGE_CURVE('',#2422,#2420,#123,.T.);
#3193=EDGE_CURVE('',#2423,#2422,#124,.T.);
#3194=EDGE_CURVE('',#2424,#2423,#125,.F.);
#3195=EDGE_CURVE('',#2424,#2425,#1172,.T.);
#3196=EDGE_CURVE('',#2425,#2425,#1910,.T.);
#3197=EDGE_CURVE('',#2426,#2424,#126,.F.);
#3198=EDGE_CURVE('',#2427,#2426,#127,.T.);
#3199=EDGE_CURVE('',#2421,#2427,#128,.T.);
#3200=EDGE_CURVE('',#2428,#2410,#1911,.T.);
#3201=EDGE_CURVE('',#2428,#2409,#88,.T.);
#3202=EDGE_CURVE('',#2406,#2429,#1912,.T.);
#3203=EDGE_CURVE('',#2429,#2405,#89,.F.);
#3204=EDGE_CURVE('',#2430,#2431,#1173,.T.);
#3205=EDGE_CURVE('',#2431,#2432,#1174,.T.);
#3206=EDGE_CURVE('',#2432,#2433,#1175,.T.);
#3207=EDGE_CURVE('',#2433,#2434,#1176,.T.);
#3208=EDGE_CURVE('',#2434,#2435,#1177,.T.);
#3209=EDGE_CURVE('',#2435,#2430,#1178,.T.);
#3210=EDGE_CURVE('',#2396,#2413,#1913,.T.);
#3211=EDGE_CURVE('',#2428,#2395,#1914,.T.);
#3212=EDGE_CURVE('',#2429,#2403,#1915,.T.);
#3213=EDGE_CURVE('',#2404,#2408,#1916,.T.);
#3214=EDGE_CURVE('',#2426,#2431,#1179,.T.);
#3215=EDGE_CURVE('',#2427,#2430,#1180,.T.);
#3216=EDGE_CURVE('',#2421,#2435,#1181,.T.);
#3217=EDGE_CURVE('',#2420,#2434,#1182,.T.);
#3218=EDGE_CURVE('',#2422,#2433,#1183,.T.);
#3219=EDGE_CURVE('',#2423,#2432,#1184,.T.);
#3220=EDGE_CURVE('',#2402,#2400,#129,.T.);
#3221=EDGE_CURVE('',#2401,#2399,#130,.T.);
#3222=ORIENTED_EDGE('',*,*,#2436,.F.);
#3223=ORIENTED_EDGE('',*,*,#2437,.T.);
#3224=ORIENTED_EDGE('',*,*,#2438,.T.);
#3225=ORIENTED_EDGE('',*,*,#2437,.F.);
#3226=ORIENTED_EDGE('',*,*,#2439,.F.);
#3227=ORIENTED_EDGE('',*,*,#2440,.T.);
#3228=ORIENTED_EDGE('',*,*,#2441,.T.);
#3229=ORIENTED_EDGE('',*,*,#2440,.F.);
#3230=ORIENTED_EDGE('',*,*,#2442,.T.);
#3231=ORIENTED_EDGE('',*,*,#2443,.T.);
#3232=ORIENTED_EDGE('',*,*,#2444,.T.);
#3233=ORIENTED_EDGE('',*,*,#2443,.F.);
#3234=ORIENTED_EDGE('',*,*,#2445,.T.);
#3235=ORIENTED_EDGE('',*,*,#2446,.T.);
#3236=ORIENTED_EDGE('',*,*,#2447,.F.);
#3237=ORIENTED_EDGE('',*,*,#2446,.F.);
#3238=ORIENTED_EDGE('',*,*,#2448,.F.);
#3239=ORIENTED_EDGE('',*,*,#2449,.T.);
#3240=ORIENTED_EDGE('',*,*,#2450,.T.);
#3241=ORIENTED_EDGE('',*,*,#2449,.F.);
#3242=ORIENTED_EDGE('',*,*,#2451,.F.);
#3243=ORIENTED_EDGE('',*,*,#2452,.T.);
#3244=ORIENTED_EDGE('',*,*,#2453,.T.);
#3245=ORIENTED_EDGE('',*,*,#2452,.F.);
#3246=ORIENTED_EDGE('',*,*,#2454,.F.);
#3247=ORIENTED_EDGE('',*,*,#2455,.T.);
#3248=ORIENTED_EDGE('',*,*,#2456,.T.);
#3249=ORIENTED_EDGE('',*,*,#2455,.F.);
#3250=ORIENTED_EDGE('',*,*,#2457,.F.);
#3251=ORIENTED_EDGE('',*,*,#2458,.T.);
#3252=ORIENTED_EDGE('',*,*,#2459,.T.);
#3253=ORIENTED_EDGE('',*,*,#2458,.F.);
#3254=ORIENTED_EDGE('',*,*,#2460,.F.);
#3255=ORIENTED_EDGE('',*,*,#2461,.T.);
#3256=ORIENTED_EDGE('',*,*,#2462,.T.);
#3257=ORIENTED_EDGE('',*,*,#2461,.F.);
#3258=ORIENTED_EDGE('',*,*,#2463,.F.);
#3259=ORIENTED_EDGE('',*,*,#2464,.T.);
#3260=ORIENTED_EDGE('',*,*,#2465,.F.);
#3261=ORIENTED_EDGE('',*,*,#2466,.T.);
#3262=ORIENTED_EDGE('',*,*,#2462,.F.);
#3263=ORIENTED_EDGE('',*,*,#2459,.F.);
#3264=ORIENTED_EDGE('',*,*,#2456,.F.);
#3265=ORIENTED_EDGE('',*,*,#2453,.F.);
#3266=ORIENTED_EDGE('',*,*,#2450,.F.);
#3267=ORIENTED_EDGE('',*,*,#2467,.F.);
#3268=ORIENTED_EDGE('',*,*,#2468,.F.);
#3269=ORIENTED_EDGE('',*,*,#2469,.F.);
#3270=ORIENTED_EDGE('',*,*,#2470,.F.);
#3271=ORIENTED_EDGE('',*,*,#2460,.T.);
#3272=ORIENTED_EDGE('',*,*,#2457,.T.);
#3273=ORIENTED_EDGE('',*,*,#2454,.T.);
#3274=ORIENTED_EDGE('',*,*,#2451,.T.);
#3275=ORIENTED_EDGE('',*,*,#2447,.T.);
#3276=ORIENTED_EDGE('',*,*,#2466,.F.);
#3277=ORIENTED_EDGE('',*,*,#2471,.F.);
#3278=ORIENTED_EDGE('',*,*,#2470,.T.);
#3279=ORIENTED_EDGE('',*,*,#2472,.T.);
#3280=ORIENTED_EDGE('',*,*,#2473,.F.);
#3281=ORIENTED_EDGE('',*,*,#2474,.T.);
#3282=ORIENTED_EDGE('',*,*,#2468,.T.);
#3283=ORIENTED_EDGE('',*,*,#2475,.T.);
#3284=ORIENTED_EDGE('',*,*,#2464,.F.);
#3285=ORIENTED_EDGE('',*,*,#2476,.F.);
#3286=ORIENTED_EDGE('',*,*,#2477,.F.);
#3287=ORIENTED_EDGE('',*,*,#2478,.F.);
#3288=ORIENTED_EDGE('',*,*,#2448,.T.);
#3289=ORIENTED_EDGE('',*,*,#2444,.F.);
#3290=ORIENTED_EDGE('',*,*,#2445,.F.);
#3291=ORIENTED_EDGE('',*,*,#2442,.F.);
#3292=ORIENTED_EDGE('',*,*,#2467,.T.);
#3293=ORIENTED_EDGE('',*,*,#2471,.T.);
#3294=ORIENTED_EDGE('',*,*,#2465,.T.);
#3295=ORIENTED_EDGE('',*,*,#2475,.F.);
#3296=ORIENTED_EDGE('',*,*,#2478,.T.);
#3297=ORIENTED_EDGE('',*,*,#2479,.F.);
#3298=ORIENTED_EDGE('',*,*,#2472,.F.);
#3299=ORIENTED_EDGE('',*,*,#2469,.T.);
#3300=ORIENTED_EDGE('',*,*,#2436,.T.);
#3301=ORIENTED_EDGE('',*,*,#2439,.T.);
#3302=ORIENTED_EDGE('',*,*,#2463,.T.);
#3303=ORIENTED_EDGE('',*,*,#2474,.F.);
#3304=ORIENTED_EDGE('',*,*,#2480,.F.);
#3305=ORIENTED_EDGE('',*,*,#2476,.T.);
#3306=ORIENTED_EDGE('',*,*,#2438,.F.);
#3307=ORIENTED_EDGE('',*,*,#2441,.F.);
#3308=ORIENTED_EDGE('',*,*,#2479,.T.);
#3309=ORIENTED_EDGE('',*,*,#2477,.T.);
#3310=ORIENTED_EDGE('',*,*,#2480,.T.);
#3311=ORIENTED_EDGE('',*,*,#2473,.T.);
#3312=ORIENTED_EDGE('',*,*,#2481,.T.);
#3313=ORIENTED_EDGE('',*,*,#2482,.T.);
#3314=ORIENTED_EDGE('',*,*,#2483,.F.);
#3315=ORIENTED_EDGE('',*,*,#2482,.F.);
#3316=ORIENTED_EDGE('',*,*,#2484,.T.);
#3317=ORIENTED_EDGE('',*,*,#2485,.T.);
#3318=ORIENTED_EDGE('',*,*,#2486,.T.);
#3319=ORIENTED_EDGE('',*,*,#2487,.T.);
#3320=ORIENTED_EDGE('',*,*,#2488,.F.);
#3321=ORIENTED_EDGE('',*,*,#2487,.F.);
#3322=ORIENTED_EDGE('',*,*,#2489,.T.);
#3323=ORIENTED_EDGE('',*,*,#2490,.F.);
#3324=ORIENTED_EDGE('',*,*,#2491,.T.);
#3325=ORIENTED_EDGE('',*,*,#2492,.T.);
#3326=ORIENTED_EDGE('',*,*,#2493,.F.);
#3327=ORIENTED_EDGE('',*,*,#2494,.F.);
#3328=ORIENTED_EDGE('',*,*,#2495,.F.);
#3329=ORIENTED_EDGE('',*,*,#2492,.F.);
#3330=ORIENTED_EDGE('',*,*,#2496,.T.);
#3331=ORIENTED_EDGE('',*,*,#2497,.T.);
#3332=ORIENTED_EDGE('',*,*,#2498,.F.);
#3333=ORIENTED_EDGE('',*,*,#2497,.F.);
#3334=ORIENTED_EDGE('',*,*,#2499,.T.);
#3335=ORIENTED_EDGE('',*,*,#2500,.T.);
#3336=ORIENTED_EDGE('',*,*,#2501,.F.);
#3337=ORIENTED_EDGE('',*,*,#2500,.F.);
#3338=ORIENTED_EDGE('',*,*,#2488,.T.);
#3339=ORIENTED_EDGE('',*,*,#2481,.F.);
#3340=ORIENTED_EDGE('',*,*,#2498,.T.);
#3341=ORIENTED_EDGE('',*,*,#2491,.F.);
#3342=ORIENTED_EDGE('',*,*,#2499,.F.);
#3343=ORIENTED_EDGE('',*,*,#2496,.F.);
#3344=ORIENTED_EDGE('',*,*,#2501,.T.);
#3345=ORIENTED_EDGE('',*,*,#2502,.F.);
#3346=ORIENTED_EDGE('',*,*,#2489,.F.);
#3347=ORIENTED_EDGE('',*,*,#2486,.F.);
#3348=ORIENTED_EDGE('',*,*,#2503,.F.);
#3349=ORIENTED_EDGE('',*,*,#2493,.T.);
#3350=ORIENTED_EDGE('',*,*,#2495,.T.);
#3351=ORIENTED_EDGE('',*,*,#2504,.F.);
#3352=ORIENTED_EDGE('',*,*,#2494,.T.);
#3353=ORIENTED_EDGE('',*,*,#2505,.F.);
#3354=ORIENTED_EDGE('',*,*,#2506,.F.);
#3355=ORIENTED_EDGE('',*,*,#2502,.T.);
#3356=ORIENTED_EDGE('',*,*,#2504,.T.);
#3357=ORIENTED_EDGE('',*,*,#2507,.F.);
#3358=ORIENTED_EDGE('',*,*,#2508,.F.);
#3359=ORIENTED_EDGE('',*,*,#2490,.T.);
#3360=ORIENTED_EDGE('',*,*,#2506,.T.);
#3361=ORIENTED_EDGE('',*,*,#2509,.F.);
#3362=ORIENTED_EDGE('',*,*,#2510,.F.);
#3363=ORIENTED_EDGE('',*,*,#2507,.T.);
#3364=ORIENTED_EDGE('',*,*,#2505,.T.);
#3365=ORIENTED_EDGE('',*,*,#2503,.T.);
#3366=ORIENTED_EDGE('',*,*,#2485,.F.);
#3367=ORIENTED_EDGE('',*,*,#2511,.F.);
#3368=ORIENTED_EDGE('',*,*,#2509,.T.);
#3369=ORIENTED_EDGE('',*,*,#2484,.F.);
#3370=ORIENTED_EDGE('',*,*,#2508,.T.);
#3371=ORIENTED_EDGE('',*,*,#2510,.T.);
#3372=ORIENTED_EDGE('',*,*,#2511,.T.);
#3373=ORIENTED_EDGE('',*,*,#2483,.T.);
#3374=ORIENTED_EDGE('',*,*,#2512,.F.);
#3375=ORIENTED_EDGE('',*,*,#2513,.T.);
#3376=ORIENTED_EDGE('',*,*,#2514,.T.);
#3377=ORIENTED_EDGE('',*,*,#2515,.T.);
#3378=ORIENTED_EDGE('',*,*,#2516,.F.);
#3379=ORIENTED_EDGE('',*,*,#2517,.F.);
#3380=ORIENTED_EDGE('',*,*,#2518,.F.);
#3381=ORIENTED_EDGE('',*,*,#2519,.F.);
#3382=ORIENTED_EDGE('',*,*,#2520,.F.);
#3383=ORIENTED_EDGE('',*,*,#2521,.F.);
#3384=ORIENTED_EDGE('',*,*,#2522,.T.);
#3385=ORIENTED_EDGE('',*,*,#2519,.T.);
#3386=ORIENTED_EDGE('',*,*,#2523,.F.);
#3387=ORIENTED_EDGE('',*,*,#2524,.F.);
#3388=ORIENTED_EDGE('',*,*,#2525,.F.);
#3389=ORIENTED_EDGE('',*,*,#2526,.F.);
#3390=ORIENTED_EDGE('',*,*,#2527,.F.);
#3391=ORIENTED_EDGE('',*,*,#2528,.F.);
#3392=ORIENTED_EDGE('',*,*,#2529,.T.);
#3393=ORIENTED_EDGE('',*,*,#2526,.T.);
#3394=ORIENTED_EDGE('',*,*,#2530,.F.);
#3395=ORIENTED_EDGE('',*,*,#2531,.F.);
#3396=ORIENTED_EDGE('',*,*,#2532,.F.);
#3397=ORIENTED_EDGE('',*,*,#2533,.F.);
#3398=ORIENTED_EDGE('',*,*,#2534,.F.);
#3399=ORIENTED_EDGE('',*,*,#2531,.T.);
#3400=ORIENTED_EDGE('',*,*,#2535,.T.);
#3401=ORIENTED_EDGE('',*,*,#2536,.F.);
#3402=ORIENTED_EDGE('',*,*,#2537,.F.);
#3403=ORIENTED_EDGE('',*,*,#2538,.F.);
#3404=ORIENTED_EDGE('',*,*,#2539,.F.);
#3405=ORIENTED_EDGE('',*,*,#2540,.F.);
#3406=ORIENTED_EDGE('',*,*,#2541,.F.);
#3407=ORIENTED_EDGE('',*,*,#2538,.T.);
#3408=ORIENTED_EDGE('',*,*,#2542,.T.);
#3409=ORIENTED_EDGE('',*,*,#2543,.F.);
#3410=ORIENTED_EDGE('',*,*,#2544,.F.);
#3411=ORIENTED_EDGE('',*,*,#2545,.F.);
#3412=ORIENTED_EDGE('',*,*,#2546,.F.);
#3413=ORIENTED_EDGE('',*,*,#2547,.F.);
#3414=ORIENTED_EDGE('',*,*,#2548,.F.);
#3415=ORIENTED_EDGE('',*,*,#2549,.F.);
#3416=ORIENTED_EDGE('',*,*,#2550,.F.);
#3417=ORIENTED_EDGE('',*,*,#2551,.F.);
#3418=ORIENTED_EDGE('',*,*,#2552,.F.);
#3419=ORIENTED_EDGE('',*,*,#2553,.F.);
#3420=ORIENTED_EDGE('',*,*,#2554,.F.);
#3421=ORIENTED_EDGE('',*,*,#2555,.F.);
#3422=ORIENTED_EDGE('',*,*,#2556,.F.);
#3423=ORIENTED_EDGE('',*,*,#2557,.F.);
#3424=ORIENTED_EDGE('',*,*,#2558,.F.);
#3425=ORIENTED_EDGE('',*,*,#2559,.F.);
#3426=ORIENTED_EDGE('',*,*,#2560,.F.);
#3427=ORIENTED_EDGE('',*,*,#2561,.F.);
#3428=ORIENTED_EDGE('',*,*,#2562,.F.);
#3429=ORIENTED_EDGE('',*,*,#2563,.F.);
#3430=ORIENTED_EDGE('',*,*,#2564,.F.);
#3431=ORIENTED_EDGE('',*,*,#2565,.F.);
#3432=ORIENTED_EDGE('',*,*,#2566,.F.);
#3433=ORIENTED_EDGE('',*,*,#2567,.F.);
#3434=ORIENTED_EDGE('',*,*,#2568,.F.);
#3435=ORIENTED_EDGE('',*,*,#2569,.F.);
#3436=ORIENTED_EDGE('',*,*,#2570,.F.);
#3437=ORIENTED_EDGE('',*,*,#2571,.F.);
#3438=ORIENTED_EDGE('',*,*,#2572,.F.);
#3439=ORIENTED_EDGE('',*,*,#2573,.F.);
#3440=ORIENTED_EDGE('',*,*,#2574,.F.);
#3441=ORIENTED_EDGE('',*,*,#2575,.F.);
#3442=ORIENTED_EDGE('',*,*,#2576,.F.);
#3443=ORIENTED_EDGE('',*,*,#2577,.F.);
#3444=ORIENTED_EDGE('',*,*,#2578,.F.);
#3445=ORIENTED_EDGE('',*,*,#2579,.F.);
#3446=ORIENTED_EDGE('',*,*,#2580,.F.);
#3447=ORIENTED_EDGE('',*,*,#2581,.F.);
#3448=ORIENTED_EDGE('',*,*,#2582,.F.);
#3449=ORIENTED_EDGE('',*,*,#2583,.F.);
#3450=ORIENTED_EDGE('',*,*,#2584,.F.);
#3451=ORIENTED_EDGE('',*,*,#2585,.T.);
#3452=ORIENTED_EDGE('',*,*,#2586,.T.);
#3453=ORIENTED_EDGE('',*,*,#2587,.T.);
#3454=ORIENTED_EDGE('',*,*,#2588,.F.);
#3455=ORIENTED_EDGE('',*,*,#2589,.T.);
#3456=ORIENTED_EDGE('',*,*,#2590,.T.);
#3457=ORIENTED_EDGE('',*,*,#2591,.T.);
#3458=ORIENTED_EDGE('',*,*,#2592,.T.);
#3459=ORIENTED_EDGE('',*,*,#2593,.T.);
#3460=ORIENTED_EDGE('',*,*,#2594,.F.);
#3461=ORIENTED_EDGE('',*,*,#2595,.T.);
#3462=ORIENTED_EDGE('',*,*,#2596,.F.);
#3463=ORIENTED_EDGE('',*,*,#2597,.T.);
#3464=ORIENTED_EDGE('',*,*,#2598,.T.);
#3465=ORIENTED_EDGE('',*,*,#2599,.T.);
#3466=ORIENTED_EDGE('',*,*,#2600,.F.);
#3467=ORIENTED_EDGE('',*,*,#2601,.T.);
#3468=ORIENTED_EDGE('',*,*,#2602,.T.);
#3469=ORIENTED_EDGE('',*,*,#2603,.T.);
#3470=ORIENTED_EDGE('',*,*,#2604,.T.);
#3471=ORIENTED_EDGE('',*,*,#2605,.T.);
#3472=ORIENTED_EDGE('',*,*,#2606,.F.);
#3473=ORIENTED_EDGE('',*,*,#2607,.T.);
#3474=ORIENTED_EDGE('',*,*,#2608,.T.);
#3475=ORIENTED_EDGE('',*,*,#2609,.T.);
#3476=ORIENTED_EDGE('',*,*,#2610,.F.);
#3477=ORIENTED_EDGE('',*,*,#2611,.T.);
#3478=ORIENTED_EDGE('',*,*,#2612,.T.);
#3479=ORIENTED_EDGE('',*,*,#2613,.T.);
#3480=ORIENTED_EDGE('',*,*,#2614,.F.);
#3481=ORIENTED_EDGE('',*,*,#2615,.T.);
#3482=ORIENTED_EDGE('',*,*,#2616,.F.);
#3483=ORIENTED_EDGE('',*,*,#2617,.T.);
#3484=ORIENTED_EDGE('',*,*,#2618,.T.);
#3485=ORIENTED_EDGE('',*,*,#2619,.T.);
#3486=ORIENTED_EDGE('',*,*,#2620,.F.);
#3487=ORIENTED_EDGE('',*,*,#2621,.T.);
#3488=ORIENTED_EDGE('',*,*,#2622,.T.);
#3489=ORIENTED_EDGE('',*,*,#2623,.T.);
#3490=ORIENTED_EDGE('',*,*,#2624,.T.);
#3491=ORIENTED_EDGE('',*,*,#2625,.T.);
#3492=ORIENTED_EDGE('',*,*,#2626,.F.);
#3493=ORIENTED_EDGE('',*,*,#2627,.T.);
#3494=ORIENTED_EDGE('',*,*,#2628,.T.);
#3495=ORIENTED_EDGE('',*,*,#2629,.T.);
#3496=ORIENTED_EDGE('',*,*,#2630,.F.);
#3497=ORIENTED_EDGE('',*,*,#2631,.T.);
#3498=ORIENTED_EDGE('',*,*,#2632,.T.);
#3499=ORIENTED_EDGE('',*,*,#2633,.T.);
#3500=ORIENTED_EDGE('',*,*,#2634,.F.);
#3501=ORIENTED_EDGE('',*,*,#2635,.T.);
#3502=ORIENTED_EDGE('',*,*,#2636,.T.);
#3503=ORIENTED_EDGE('',*,*,#2637,.T.);
#3504=ORIENTED_EDGE('',*,*,#2638,.F.);
#3505=ORIENTED_EDGE('',*,*,#2639,.T.);
#3506=ORIENTED_EDGE('',*,*,#2640,.T.);
#3507=ORIENTED_EDGE('',*,*,#2641,.T.);
#3508=ORIENTED_EDGE('',*,*,#2642,.F.);
#3509=ORIENTED_EDGE('',*,*,#2521,.T.);
#3510=ORIENTED_EDGE('',*,*,#2643,.T.);
#3511=ORIENTED_EDGE('',*,*,#2644,.T.);
#3512=ORIENTED_EDGE('',*,*,#2645,.F.);
#3513=ORIENTED_EDGE('',*,*,#2528,.T.);
#3514=ORIENTED_EDGE('',*,*,#2646,.F.);
#3515=ORIENTED_EDGE('',*,*,#2647,.T.);
#3516=ORIENTED_EDGE('',*,*,#2648,.T.);
#3517=ORIENTED_EDGE('',*,*,#2543,.T.);
#3518=ORIENTED_EDGE('',*,*,#2649,.F.);
#3519=ORIENTED_EDGE('',*,*,#2650,.T.);
#3520=ORIENTED_EDGE('',*,*,#2651,.T.);
#3521=ORIENTED_EDGE('',*,*,#2652,.T.);
#3522=ORIENTED_EDGE('',*,*,#2653,.F.);
#3523=ORIENTED_EDGE('',*,*,#2654,.T.);
#3524=ORIENTED_EDGE('',*,*,#2655,.T.);
#3525=ORIENTED_EDGE('',*,*,#2656,.T.);
#3526=ORIENTED_EDGE('',*,*,#2657,.T.);
#3527=ORIENTED_EDGE('',*,*,#2658,.T.);
#3528=ORIENTED_EDGE('',*,*,#2659,.F.);
#3529=ORIENTED_EDGE('',*,*,#2660,.T.);
#3530=ORIENTED_EDGE('',*,*,#2661,.F.);
#3531=ORIENTED_EDGE('',*,*,#2662,.T.);
#3532=ORIENTED_EDGE('',*,*,#2663,.T.);
#3533=ORIENTED_EDGE('',*,*,#2664,.T.);
#3534=ORIENTED_EDGE('',*,*,#2665,.F.);
#3535=ORIENTED_EDGE('',*,*,#2666,.T.);
#3536=ORIENTED_EDGE('',*,*,#2667,.T.);
#3537=ORIENTED_EDGE('',*,*,#2668,.T.);
#3538=ORIENTED_EDGE('',*,*,#2669,.F.);
#3539=ORIENTED_EDGE('',*,*,#2670,.T.);
#3540=ORIENTED_EDGE('',*,*,#2671,.T.);
#3541=ORIENTED_EDGE('',*,*,#2672,.T.);
#3542=ORIENTED_EDGE('',*,*,#2673,.F.);
#3543=ORIENTED_EDGE('',*,*,#2674,.T.);
#3544=ORIENTED_EDGE('',*,*,#2675,.T.);
#3545=ORIENTED_EDGE('',*,*,#2676,.T.);
#3546=ORIENTED_EDGE('',*,*,#2677,.F.);
#3547=ORIENTED_EDGE('',*,*,#2678,.T.);
#3548=ORIENTED_EDGE('',*,*,#2679,.T.);
#3549=ORIENTED_EDGE('',*,*,#2680,.T.);
#3550=ORIENTED_EDGE('',*,*,#2681,.T.);
#3551=ORIENTED_EDGE('',*,*,#2682,.T.);
#3552=ORIENTED_EDGE('',*,*,#2683,.F.);
#3553=ORIENTED_EDGE('',*,*,#2684,.T.);
#3554=ORIENTED_EDGE('',*,*,#2685,.T.);
#3555=ORIENTED_EDGE('',*,*,#2686,.T.);
#3556=ORIENTED_EDGE('',*,*,#2687,.F.);
#3557=ORIENTED_EDGE('',*,*,#2688,.T.);
#3558=ORIENTED_EDGE('',*,*,#2689,.T.);
#3559=ORIENTED_EDGE('',*,*,#2690,.T.);
#3560=ORIENTED_EDGE('',*,*,#2691,.F.);
#3561=ORIENTED_EDGE('',*,*,#2692,.T.);
#3562=ORIENTED_EDGE('',*,*,#2693,.F.);
#3563=ORIENTED_EDGE('',*,*,#2694,.T.);
#3564=ORIENTED_EDGE('',*,*,#2695,.T.);
#3565=ORIENTED_EDGE('',*,*,#2696,.T.);
#3566=ORIENTED_EDGE('',*,*,#2590,.F.);
#3567=ORIENTED_EDGE('',*,*,#2697,.T.);
#3568=ORIENTED_EDGE('',*,*,#2698,.T.);
#3569=ORIENTED_EDGE('',*,*,#2699,.T.);
#3570=ORIENTED_EDGE('',*,*,#2700,.T.);
#3571=ORIENTED_EDGE('',*,*,#2701,.T.);
#3572=ORIENTED_EDGE('',*,*,#2592,.F.);
#3573=ORIENTED_EDGE('',*,*,#2702,.T.);
#3574=ORIENTED_EDGE('',*,*,#2703,.T.);
#3575=ORIENTED_EDGE('',*,*,#2704,.T.);
#3576=ORIENTED_EDGE('',*,*,#2705,.T.);
#3577=ORIENTED_EDGE('',*,*,#2706,.T.);
#3578=ORIENTED_EDGE('',*,*,#2604,.F.);
#3579=ORIENTED_EDGE('',*,*,#2707,.T.);
#3580=ORIENTED_EDGE('',*,*,#2708,.T.);
#3581=ORIENTED_EDGE('',*,*,#2709,.T.);
#3582=ORIENTED_EDGE('',*,*,#2710,.T.);
#3583=ORIENTED_EDGE('',*,*,#2711,.T.);
#3584=ORIENTED_EDGE('',*,*,#2608,.F.);
#3585=ORIENTED_EDGE('',*,*,#2712,.T.);
#3586=ORIENTED_EDGE('',*,*,#2713,.T.);
#3587=ORIENTED_EDGE('',*,*,#2714,.T.);
#3588=ORIENTED_EDGE('',*,*,#2715,.T.);
#3589=ORIENTED_EDGE('',*,*,#2716,.T.);
#3590=ORIENTED_EDGE('',*,*,#2586,.F.);
#3591=ORIENTED_EDGE('',*,*,#2717,.T.);
#3592=ORIENTED_EDGE('',*,*,#2718,.T.);
#3593=ORIENTED_EDGE('',*,*,#2719,.T.);
#3594=ORIENTED_EDGE('',*,*,#2720,.T.);
#3595=ORIENTED_EDGE('',*,*,#2721,.T.);
#3596=ORIENTED_EDGE('',*,*,#2612,.F.);
#3597=ORIENTED_EDGE('',*,*,#2722,.T.);
#3598=ORIENTED_EDGE('',*,*,#2723,.T.);
#3599=ORIENTED_EDGE('',*,*,#2724,.T.);
#3600=ORIENTED_EDGE('',*,*,#2725,.T.);
#3601=ORIENTED_EDGE('',*,*,#2726,.T.);
#3602=ORIENTED_EDGE('',*,*,#2624,.F.);
#3603=ORIENTED_EDGE('',*,*,#2727,.T.);
#3604=ORIENTED_EDGE('',*,*,#2728,.T.);
#3605=ORIENTED_EDGE('',*,*,#2729,.T.);
#3606=ORIENTED_EDGE('',*,*,#2730,.T.);
#3607=ORIENTED_EDGE('',*,*,#2731,.T.);
#3608=ORIENTED_EDGE('',*,*,#2628,.F.);
#3609=ORIENTED_EDGE('',*,*,#2732,.T.);
#3610=ORIENTED_EDGE('',*,*,#2733,.T.);
#3611=ORIENTED_EDGE('',*,*,#2734,.T.);
#3612=ORIENTED_EDGE('',*,*,#2735,.T.);
#3613=ORIENTED_EDGE('',*,*,#2736,.T.);
#3614=ORIENTED_EDGE('',*,*,#2622,.F.);
#3615=ORIENTED_EDGE('',*,*,#2737,.T.);
#3616=ORIENTED_EDGE('',*,*,#2738,.T.);
#3617=ORIENTED_EDGE('',*,*,#2739,.T.);
#3618=ORIENTED_EDGE('',*,*,#2740,.T.);
#3619=ORIENTED_EDGE('',*,*,#2741,.T.);
#3620=ORIENTED_EDGE('',*,*,#2618,.F.);
#3621=ORIENTED_EDGE('',*,*,#2742,.T.);
#3622=ORIENTED_EDGE('',*,*,#2743,.T.);
#3623=ORIENTED_EDGE('',*,*,#2744,.T.);
#3624=ORIENTED_EDGE('',*,*,#2745,.T.);
#3625=ORIENTED_EDGE('',*,*,#2746,.T.);
#3626=ORIENTED_EDGE('',*,*,#2632,.F.);
#3627=ORIENTED_EDGE('',*,*,#2747,.T.);
#3628=ORIENTED_EDGE('',*,*,#2748,.T.);
#3629=ORIENTED_EDGE('',*,*,#2749,.T.);
#3630=ORIENTED_EDGE('',*,*,#2750,.T.);
#3631=ORIENTED_EDGE('',*,*,#2751,.T.);
#3632=ORIENTED_EDGE('',*,*,#2636,.F.);
#3633=ORIENTED_EDGE('',*,*,#2752,.T.);
#3634=ORIENTED_EDGE('',*,*,#2753,.T.);
#3635=ORIENTED_EDGE('',*,*,#2754,.T.);
#3636=ORIENTED_EDGE('',*,*,#2755,.T.);
#3637=ORIENTED_EDGE('',*,*,#2756,.T.);
#3638=ORIENTED_EDGE('',*,*,#2640,.F.);
#3639=ORIENTED_EDGE('',*,*,#2520,.T.);
#3640=ORIENTED_EDGE('',*,*,#2518,.T.);
#3641=ORIENTED_EDGE('',*,*,#2757,.T.);
#3642=ORIENTED_EDGE('',*,*,#2758,.T.);
#3643=ORIENTED_EDGE('',*,*,#2759,.T.);
#3644=ORIENTED_EDGE('',*,*,#2643,.F.);
#3645=ORIENTED_EDGE('',*,*,#2527,.T.);
#3646=ORIENTED_EDGE('',*,*,#2525,.T.);
#3647=ORIENTED_EDGE('',*,*,#2760,.T.);
#3648=ORIENTED_EDGE('',*,*,#2761,.T.);
#3649=ORIENTED_EDGE('',*,*,#2762,.T.);
#3650=ORIENTED_EDGE('',*,*,#2681,.F.);
#3651=ORIENTED_EDGE('',*,*,#2763,.T.);
#3652=ORIENTED_EDGE('',*,*,#2574,.T.);
#3653=ORIENTED_EDGE('',*,*,#2764,.T.);
#3654=ORIENTED_EDGE('',*,*,#2765,.T.);
#3655=ORIENTED_EDGE('',*,*,#2766,.T.);
#3656=ORIENTED_EDGE('',*,*,#2679,.F.);
#3657=ORIENTED_EDGE('',*,*,#2767,.T.);
#3658=ORIENTED_EDGE('',*,*,#2570,.T.);
#3659=ORIENTED_EDGE('',*,*,#2768,.T.);
#3660=ORIENTED_EDGE('',*,*,#2769,.T.);
#3661=ORIENTED_EDGE('',*,*,#2770,.T.);
#3662=ORIENTED_EDGE('',*,*,#2685,.F.);
#3663=ORIENTED_EDGE('',*,*,#2771,.T.);
#3664=ORIENTED_EDGE('',*,*,#2578,.T.);
#3665=ORIENTED_EDGE('',*,*,#2772,.T.);
#3666=ORIENTED_EDGE('',*,*,#2773,.T.);
#3667=ORIENTED_EDGE('',*,*,#2774,.T.);
#3668=ORIENTED_EDGE('',*,*,#2689,.F.);
#3669=ORIENTED_EDGE('',*,*,#2775,.T.);
#3670=ORIENTED_EDGE('',*,*,#2582,.T.);
#3671=ORIENTED_EDGE('',*,*,#2776,.T.);
#3672=ORIENTED_EDGE('',*,*,#2777,.T.);
#3673=ORIENTED_EDGE('',*,*,#2778,.T.);
#3674=ORIENTED_EDGE('',*,*,#2675,.F.);
#3675=ORIENTED_EDGE('',*,*,#2779,.T.);
#3676=ORIENTED_EDGE('',*,*,#2566,.T.);
#3677=ORIENTED_EDGE('',*,*,#2780,.T.);
#3678=ORIENTED_EDGE('',*,*,#2781,.T.);
#3679=ORIENTED_EDGE('',*,*,#2782,.T.);
#3680=ORIENTED_EDGE('',*,*,#2671,.F.);
#3681=ORIENTED_EDGE('',*,*,#2783,.T.);
#3682=ORIENTED_EDGE('',*,*,#2784,.T.);
#3683=ORIENTED_EDGE('',*,*,#2785,.T.);
#3684=ORIENTED_EDGE('',*,*,#2562,.T.);
#3685=ORIENTED_EDGE('',*,*,#2786,.T.);
#3686=ORIENTED_EDGE('',*,*,#2667,.F.);
#3687=ORIENTED_EDGE('',*,*,#2787,.T.);
#3688=ORIENTED_EDGE('',*,*,#2788,.T.);
#3689=ORIENTED_EDGE('',*,*,#2789,.T.);
#3690=ORIENTED_EDGE('',*,*,#2558,.T.);
#3691=ORIENTED_EDGE('',*,*,#2790,.T.);
#3692=ORIENTED_EDGE('',*,*,#2663,.F.);
#3693=ORIENTED_EDGE('',*,*,#2791,.T.);
#3694=ORIENTED_EDGE('',*,*,#2792,.T.);
#3695=ORIENTED_EDGE('',*,*,#2793,.T.);
#3696=ORIENTED_EDGE('',*,*,#2554,.T.);
#3697=ORIENTED_EDGE('',*,*,#2794,.T.);
#3698=ORIENTED_EDGE('',*,*,#2655,.F.);
#3699=ORIENTED_EDGE('',*,*,#2795,.T.);
#3700=ORIENTED_EDGE('',*,*,#2796,.T.);
#3701=ORIENTED_EDGE('',*,*,#2797,.T.);
#3702=ORIENTED_EDGE('',*,*,#2546,.T.);
#3703=ORIENTED_EDGE('',*,*,#2798,.T.);
#3704=ORIENTED_EDGE('',*,*,#2657,.F.);
#3705=ORIENTED_EDGE('',*,*,#2799,.T.);
#3706=ORIENTED_EDGE('',*,*,#2800,.T.);
#3707=ORIENTED_EDGE('',*,*,#2801,.T.);
#3708=ORIENTED_EDGE('',*,*,#2550,.T.);
#3709=ORIENTED_EDGE('',*,*,#2802,.T.);
#3710=ORIENTED_EDGE('',*,*,#2651,.F.);
#3711=ORIENTED_EDGE('',*,*,#2803,.T.);
#3712=ORIENTED_EDGE('',*,*,#2804,.T.);
#3713=ORIENTED_EDGE('',*,*,#2805,.T.);
#3714=ORIENTED_EDGE('',*,*,#2539,.T.);
#3715=ORIENTED_EDGE('',*,*,#2541,.T.);
#3716=ORIENTED_EDGE('',*,*,#2648,.F.);
#3717=ORIENTED_EDGE('',*,*,#2806,.T.);
#3718=ORIENTED_EDGE('',*,*,#2807,.T.);
#3719=ORIENTED_EDGE('',*,*,#2808,.T.);
#3720=ORIENTED_EDGE('',*,*,#2532,.T.);
#3721=ORIENTED_EDGE('',*,*,#2534,.T.);
#3722=ORIENTED_EDGE('',*,*,#2809,.F.);
#3723=ORIENTED_EDGE('',*,*,#2810,.T.);
#3724=ORIENTED_EDGE('',*,*,#2811,.T.);
#3725=ORIENTED_EDGE('',*,*,#2812,.T.);
#3726=ORIENTED_EDGE('',*,*,#2813,.T.);
#3727=ORIENTED_EDGE('',*,*,#2814,.T.);
#3728=ORIENTED_EDGE('',*,*,#2695,.F.);
#3729=ORIENTED_EDGE('',*,*,#2815,.T.);
#3730=ORIENTED_EDGE('',*,*,#2816,.T.);
#3731=ORIENTED_EDGE('',*,*,#2817,.T.);
#3732=ORIENTED_EDGE('',*,*,#2818,.T.);
#3733=ORIENTED_EDGE('',*,*,#2819,.T.);
#3734=ORIENTED_EDGE('',*,*,#2602,.F.);
#3735=ORIENTED_EDGE('',*,*,#2820,.T.);
#3736=ORIENTED_EDGE('',*,*,#2821,.T.);
#3737=ORIENTED_EDGE('',*,*,#2822,.T.);
#3738=ORIENTED_EDGE('',*,*,#2823,.T.);
#3739=ORIENTED_EDGE('',*,*,#2824,.T.);
#3740=ORIENTED_EDGE('',*,*,#2598,.F.);
#3741=ORIENTED_EDGE('',*,*,#2825,.T.);
#3742=ORIENTED_EDGE('',*,*,#2826,.T.);
#3743=ORIENTED_EDGE('',*,*,#2827,.T.);
#3744=ORIENTED_EDGE('',*,*,#2828,.T.);
#3745=ORIENTED_EDGE('',*,*,#2829,.T.);
#3746=ORIENTED_EDGE('',*,*,#2830,.T.);
#3747=ORIENTED_EDGE('',*,*,#2831,.T.);
#3748=ORIENTED_EDGE('',*,*,#2512,.T.);
#3749=ORIENTED_EDGE('',*,*,#2832,.T.);
#3750=ORIENTED_EDGE('',*,*,#2833,.F.);
#3751=ORIENTED_EDGE('',*,*,#2588,.T.);
#3752=ORIENTED_EDGE('',*,*,#2834,.F.);
#3753=ORIENTED_EDGE('',*,*,#2835,.T.);
#3754=ORIENTED_EDGE('',*,*,#2836,.F.);
#3755=ORIENTED_EDGE('',*,*,#2837,.T.);
#3756=ORIENTED_EDGE('',*,*,#2838,.F.);
#3757=ORIENTED_EDGE('',*,*,#2596,.T.);
#3758=ORIENTED_EDGE('',*,*,#2839,.F.);
#3759=ORIENTED_EDGE('',*,*,#2840,.T.);
#3760=ORIENTED_EDGE('',*,*,#2841,.F.);
#3761=ORIENTED_EDGE('',*,*,#2842,.T.);
#3762=ORIENTED_EDGE('',*,*,#2843,.F.);
#3763=ORIENTED_EDGE('',*,*,#2600,.T.);
#3764=ORIENTED_EDGE('',*,*,#2844,.F.);
#3765=ORIENTED_EDGE('',*,*,#2845,.T.);
#3766=ORIENTED_EDGE('',*,*,#2846,.F.);
#3767=ORIENTED_EDGE('',*,*,#2847,.T.);
#3768=ORIENTED_EDGE('',*,*,#2848,.F.);
#3769=ORIENTED_EDGE('',*,*,#2693,.T.);
#3770=ORIENTED_EDGE('',*,*,#2849,.F.);
#3771=ORIENTED_EDGE('',*,*,#2850,.T.);
#3772=ORIENTED_EDGE('',*,*,#2851,.F.);
#3773=ORIENTED_EDGE('',*,*,#2852,.T.);
#3774=ORIENTED_EDGE('',*,*,#2853,.F.);
#3775=ORIENTED_EDGE('',*,*,#2854,.T.);
#3776=ORIENTED_EDGE('',*,*,#2535,.F.);
#3777=ORIENTED_EDGE('',*,*,#2530,.T.);
#3778=ORIENTED_EDGE('',*,*,#2855,.F.);
#3779=ORIENTED_EDGE('',*,*,#2856,.T.);
#3780=ORIENTED_EDGE('',*,*,#2857,.F.);
#3781=ORIENTED_EDGE('',*,*,#2646,.T.);
#3782=ORIENTED_EDGE('',*,*,#2542,.F.);
#3783=ORIENTED_EDGE('',*,*,#2537,.T.);
#3784=ORIENTED_EDGE('',*,*,#2858,.F.);
#3785=ORIENTED_EDGE('',*,*,#2859,.T.);
#3786=ORIENTED_EDGE('',*,*,#2860,.F.);
#3787=ORIENTED_EDGE('',*,*,#2649,.T.);
#3788=ORIENTED_EDGE('',*,*,#2861,.F.);
#3789=ORIENTED_EDGE('',*,*,#2548,.T.);
#3790=ORIENTED_EDGE('',*,*,#2862,.F.);
#3791=ORIENTED_EDGE('',*,*,#2863,.T.);
#3792=ORIENTED_EDGE('',*,*,#2864,.F.);
#3793=ORIENTED_EDGE('',*,*,#2659,.T.);
#3794=ORIENTED_EDGE('',*,*,#2865,.F.);
#3795=ORIENTED_EDGE('',*,*,#2544,.T.);
#3796=ORIENTED_EDGE('',*,*,#2866,.F.);
#3797=ORIENTED_EDGE('',*,*,#2867,.T.);
#3798=ORIENTED_EDGE('',*,*,#2868,.F.);
#3799=ORIENTED_EDGE('',*,*,#2653,.T.);
#3800=ORIENTED_EDGE('',*,*,#2869,.F.);
#3801=ORIENTED_EDGE('',*,*,#2552,.T.);
#3802=ORIENTED_EDGE('',*,*,#2870,.F.);
#3803=ORIENTED_EDGE('',*,*,#2871,.T.);
#3804=ORIENTED_EDGE('',*,*,#2872,.F.);
#3805=ORIENTED_EDGE('',*,*,#2661,.T.);
#3806=ORIENTED_EDGE('',*,*,#2873,.F.);
#3807=ORIENTED_EDGE('',*,*,#2556,.T.);
#3808=ORIENTED_EDGE('',*,*,#2874,.F.);
#3809=ORIENTED_EDGE('',*,*,#2875,.T.);
#3810=ORIENTED_EDGE('',*,*,#2876,.F.);
#3811=ORIENTED_EDGE('',*,*,#2665,.T.);
#3812=ORIENTED_EDGE('',*,*,#2877,.F.);
#3813=ORIENTED_EDGE('',*,*,#2560,.T.);
#3814=ORIENTED_EDGE('',*,*,#2878,.F.);
#3815=ORIENTED_EDGE('',*,*,#2879,.T.);
#3816=ORIENTED_EDGE('',*,*,#2880,.F.);
#3817=ORIENTED_EDGE('',*,*,#2669,.T.);
#3818=ORIENTED_EDGE('',*,*,#2881,.F.);
#3819=ORIENTED_EDGE('',*,*,#2882,.T.);
#3820=ORIENTED_EDGE('',*,*,#2883,.F.);
#3821=ORIENTED_EDGE('',*,*,#2564,.T.);
#3822=ORIENTED_EDGE('',*,*,#2884,.F.);
#3823=ORIENTED_EDGE('',*,*,#2673,.T.);
#3824=ORIENTED_EDGE('',*,*,#2885,.F.);
#3825=ORIENTED_EDGE('',*,*,#2886,.T.);
#3826=ORIENTED_EDGE('',*,*,#2887,.F.);
#3827=ORIENTED_EDGE('',*,*,#2580,.T.);
#3828=ORIENTED_EDGE('',*,*,#2888,.F.);
#3829=ORIENTED_EDGE('',*,*,#2691,.T.);
#3830=ORIENTED_EDGE('',*,*,#2889,.F.);
#3831=ORIENTED_EDGE('',*,*,#2890,.T.);
#3832=ORIENTED_EDGE('',*,*,#2891,.F.);
#3833=ORIENTED_EDGE('',*,*,#2576,.T.);
#3834=ORIENTED_EDGE('',*,*,#2892,.F.);
#3835=ORIENTED_EDGE('',*,*,#2687,.T.);
#3836=ORIENTED_EDGE('',*,*,#2893,.F.);
#3837=ORIENTED_EDGE('',*,*,#2894,.T.);
#3838=ORIENTED_EDGE('',*,*,#2895,.F.);
#3839=ORIENTED_EDGE('',*,*,#2568,.T.);
#3840=ORIENTED_EDGE('',*,*,#2896,.F.);
#3841=ORIENTED_EDGE('',*,*,#2677,.T.);
#3842=ORIENTED_EDGE('',*,*,#2897,.F.);
#3843=ORIENTED_EDGE('',*,*,#2898,.T.);
#3844=ORIENTED_EDGE('',*,*,#2899,.F.);
#3845=ORIENTED_EDGE('',*,*,#2572,.T.);
#3846=ORIENTED_EDGE('',*,*,#2900,.F.);
#3847=ORIENTED_EDGE('',*,*,#2683,.T.);
#3848=ORIENTED_EDGE('',*,*,#2901,.F.);
#3849=ORIENTED_EDGE('',*,*,#2902,.T.);
#3850=ORIENTED_EDGE('',*,*,#2903,.F.);
#3851=ORIENTED_EDGE('',*,*,#2523,.T.);
#3852=ORIENTED_EDGE('',*,*,#2529,.F.);
#3853=ORIENTED_EDGE('',*,*,#2645,.T.);
#3854=ORIENTED_EDGE('',*,*,#2904,.F.);
#3855=ORIENTED_EDGE('',*,*,#2905,.T.);
#3856=ORIENTED_EDGE('',*,*,#2906,.F.);
#3857=ORIENTED_EDGE('',*,*,#2516,.T.);
#3858=ORIENTED_EDGE('',*,*,#2522,.F.);
#3859=ORIENTED_EDGE('',*,*,#2642,.T.);
#3860=ORIENTED_EDGE('',*,*,#2907,.F.);
#3861=ORIENTED_EDGE('',*,*,#2908,.T.);
#3862=ORIENTED_EDGE('',*,*,#2909,.F.);
#3863=ORIENTED_EDGE('',*,*,#2910,.T.);
#3864=ORIENTED_EDGE('',*,*,#2911,.F.);
#3865=ORIENTED_EDGE('',*,*,#2638,.T.);
#3866=ORIENTED_EDGE('',*,*,#2912,.F.);
#3867=ORIENTED_EDGE('',*,*,#2913,.T.);
#3868=ORIENTED_EDGE('',*,*,#2914,.F.);
#3869=ORIENTED_EDGE('',*,*,#2915,.T.);
#3870=ORIENTED_EDGE('',*,*,#2916,.F.);
#3871=ORIENTED_EDGE('',*,*,#2634,.T.);
#3872=ORIENTED_EDGE('',*,*,#2917,.F.);
#3873=ORIENTED_EDGE('',*,*,#2918,.T.);
#3874=ORIENTED_EDGE('',*,*,#2919,.F.);
#3875=ORIENTED_EDGE('',*,*,#2920,.T.);
#3876=ORIENTED_EDGE('',*,*,#2921,.F.);
#3877=ORIENTED_EDGE('',*,*,#2616,.T.);
#3878=ORIENTED_EDGE('',*,*,#2922,.F.);
#3879=ORIENTED_EDGE('',*,*,#2923,.T.);
#3880=ORIENTED_EDGE('',*,*,#2924,.F.);
#3881=ORIENTED_EDGE('',*,*,#2925,.T.);
#3882=ORIENTED_EDGE('',*,*,#2926,.F.);
#3883=ORIENTED_EDGE('',*,*,#2620,.T.);
#3884=ORIENTED_EDGE('',*,*,#2927,.F.);
#3885=ORIENTED_EDGE('',*,*,#2928,.T.);
#3886=ORIENTED_EDGE('',*,*,#2929,.F.);
#3887=ORIENTED_EDGE('',*,*,#2930,.T.);
#3888=ORIENTED_EDGE('',*,*,#2931,.F.);
#3889=ORIENTED_EDGE('',*,*,#2630,.T.);
#3890=ORIENTED_EDGE('',*,*,#2932,.F.);
#3891=ORIENTED_EDGE('',*,*,#2933,.T.);
#3892=ORIENTED_EDGE('',*,*,#2934,.F.);
#3893=ORIENTED_EDGE('',*,*,#2935,.T.);
#3894=ORIENTED_EDGE('',*,*,#2936,.F.);
#3895=ORIENTED_EDGE('',*,*,#2626,.T.);
#3896=ORIENTED_EDGE('',*,*,#2937,.F.);
#3897=ORIENTED_EDGE('',*,*,#2938,.T.);
#3898=ORIENTED_EDGE('',*,*,#2939,.F.);
#3899=ORIENTED_EDGE('',*,*,#2940,.T.);
#3900=ORIENTED_EDGE('',*,*,#2941,.F.);
#3901=ORIENTED_EDGE('',*,*,#2614,.T.);
#3902=ORIENTED_EDGE('',*,*,#2942,.F.);
#3903=ORIENTED_EDGE('',*,*,#2943,.T.);
#3904=ORIENTED_EDGE('',*,*,#2944,.F.);
#3905=ORIENTED_EDGE('',*,*,#2945,.T.);
#3906=ORIENTED_EDGE('',*,*,#2946,.F.);
#3907=ORIENTED_EDGE('',*,*,#2584,.T.);
#3908=ORIENTED_EDGE('',*,*,#2947,.F.);
#3909=ORIENTED_EDGE('',*,*,#2948,.T.);
#3910=ORIENTED_EDGE('',*,*,#2949,.F.);
#3911=ORIENTED_EDGE('',*,*,#2950,.T.);
#3912=ORIENTED_EDGE('',*,*,#2951,.F.);
#3913=ORIENTED_EDGE('',*,*,#2610,.T.);
#3914=ORIENTED_EDGE('',*,*,#2952,.F.);
#3915=ORIENTED_EDGE('',*,*,#2953,.T.);
#3916=ORIENTED_EDGE('',*,*,#2954,.F.);
#3917=ORIENTED_EDGE('',*,*,#2955,.T.);
#3918=ORIENTED_EDGE('',*,*,#2956,.F.);
#3919=ORIENTED_EDGE('',*,*,#2606,.T.);
#3920=ORIENTED_EDGE('',*,*,#2957,.F.);
#3921=ORIENTED_EDGE('',*,*,#2958,.T.);
#3922=ORIENTED_EDGE('',*,*,#2959,.F.);
#3923=ORIENTED_EDGE('',*,*,#2960,.T.);
#3924=ORIENTED_EDGE('',*,*,#2961,.F.);
#3925=ORIENTED_EDGE('',*,*,#2594,.T.);
#3926=ORIENTED_EDGE('',*,*,#2962,.F.);
#3927=ORIENTED_EDGE('',*,*,#2963,.T.);
#3928=ORIENTED_EDGE('',*,*,#2964,.F.);
#3929=ORIENTED_EDGE('',*,*,#2965,.T.);
#3930=ORIENTED_EDGE('',*,*,#2966,.F.);
#3931=ORIENTED_EDGE('',*,*,#2967,.F.);
#3932=ORIENTED_EDGE('',*,*,#2968,.F.);
#3933=ORIENTED_EDGE('',*,*,#2514,.F.);
#3934=ORIENTED_EDGE('',*,*,#2809,.T.);
#3935=ORIENTED_EDGE('',*,*,#2536,.T.);
#3936=ORIENTED_EDGE('',*,*,#2854,.F.);
#3937=ORIENTED_EDGE('',*,*,#2969,.T.);
#3938=ORIENTED_EDGE('',*,*,#2814,.F.);
#3939=ORIENTED_EDGE('',*,*,#2970,.T.);
#3940=ORIENTED_EDGE('',*,*,#2849,.T.);
#3941=ORIENTED_EDGE('',*,*,#2696,.F.);
#3942=ORIENTED_EDGE('',*,*,#2853,.T.);
#3943=ORIENTED_EDGE('',*,*,#2971,.T.);
#3944=ORIENTED_EDGE('',*,*,#2810,.F.);
#3945=ORIENTED_EDGE('',*,*,#2969,.F.);
#3946=ORIENTED_EDGE('',*,*,#2851,.T.);
#3947=ORIENTED_EDGE('',*,*,#2972,.T.);
#3948=ORIENTED_EDGE('',*,*,#2812,.F.);
#3949=ORIENTED_EDGE('',*,*,#2973,.T.);
#3950=ORIENTED_EDGE('',*,*,#2813,.F.);
#3951=ORIENTED_EDGE('',*,*,#2972,.F.);
#3952=ORIENTED_EDGE('',*,*,#2850,.F.);
#3953=ORIENTED_EDGE('',*,*,#2970,.F.);
#3954=ORIENTED_EDGE('',*,*,#2811,.F.);
#3955=ORIENTED_EDGE('',*,*,#2971,.F.);
#3956=ORIENTED_EDGE('',*,*,#2852,.F.);
#3957=ORIENTED_EDGE('',*,*,#2973,.F.);
#3958=ORIENTED_EDGE('',*,*,#2848,.T.);
#3959=ORIENTED_EDGE('',*,*,#2974,.T.);
#3960=ORIENTED_EDGE('',*,*,#2815,.F.);
#3961=ORIENTED_EDGE('',*,*,#2694,.F.);
#3962=ORIENTED_EDGE('',*,*,#2819,.F.);
#3963=ORIENTED_EDGE('',*,*,#2975,.T.);
#3964=ORIENTED_EDGE('',*,*,#2844,.T.);
#3965=ORIENTED_EDGE('',*,*,#2603,.F.);
#3966=ORIENTED_EDGE('',*,*,#2818,.F.);
#3967=ORIENTED_EDGE('',*,*,#2976,.F.);
#3968=ORIENTED_EDGE('',*,*,#2845,.F.);
#3969=ORIENTED_EDGE('',*,*,#2975,.F.);
#3970=ORIENTED_EDGE('',*,*,#2846,.T.);
#3971=ORIENTED_EDGE('',*,*,#2976,.T.);
#3972=ORIENTED_EDGE('',*,*,#2817,.F.);
#3973=ORIENTED_EDGE('',*,*,#2977,.T.);
#3974=ORIENTED_EDGE('',*,*,#2816,.F.);
#3975=ORIENTED_EDGE('',*,*,#2974,.F.);
#3976=ORIENTED_EDGE('',*,*,#2847,.F.);
#3977=ORIENTED_EDGE('',*,*,#2977,.F.);
#3978=ORIENTED_EDGE('',*,*,#2888,.T.);
#3979=ORIENTED_EDGE('',*,*,#2583,.T.);
#3980=ORIENTED_EDGE('',*,*,#2775,.F.);
#3981=ORIENTED_EDGE('',*,*,#2692,.F.);
#3982=ORIENTED_EDGE('',*,*,#2778,.F.);
#3983=ORIENTED_EDGE('',*,*,#2978,.T.);
#3984=ORIENTED_EDGE('',*,*,#2885,.T.);
#3985=ORIENTED_EDGE('',*,*,#2676,.F.);
#3986=ORIENTED_EDGE('',*,*,#2777,.F.);
#3987=ORIENTED_EDGE('',*,*,#2979,.F.);
#3988=ORIENTED_EDGE('',*,*,#2886,.F.);
#3989=ORIENTED_EDGE('',*,*,#2978,.F.);
#3990=ORIENTED_EDGE('',*,*,#2887,.T.);
#3991=ORIENTED_EDGE('',*,*,#2979,.T.);
#3992=ORIENTED_EDGE('',*,*,#2776,.F.);
#3993=ORIENTED_EDGE('',*,*,#2581,.T.);
#3994=ORIENTED_EDGE('',*,*,#2892,.T.);
#3995=ORIENTED_EDGE('',*,*,#2579,.T.);
#3996=ORIENTED_EDGE('',*,*,#2771,.F.);
#3997=ORIENTED_EDGE('',*,*,#2688,.F.);
#3998=ORIENTED_EDGE('',*,*,#2774,.F.);
#3999=ORIENTED_EDGE('',*,*,#2980,.T.);
#4000=ORIENTED_EDGE('',*,*,#2889,.T.);
#4001=ORIENTED_EDGE('',*,*,#2690,.F.);
#4002=ORIENTED_EDGE('',*,*,#2773,.F.);
#4003=ORIENTED_EDGE('',*,*,#2981,.F.);
#4004=ORIENTED_EDGE('',*,*,#2890,.F.);
#4005=ORIENTED_EDGE('',*,*,#2980,.F.);
#4006=ORIENTED_EDGE('',*,*,#2891,.T.);
#4007=ORIENTED_EDGE('',*,*,#2981,.T.);
#4008=ORIENTED_EDGE('',*,*,#2772,.F.);
#4009=ORIENTED_EDGE('',*,*,#2577,.T.);
#4010=ORIENTED_EDGE('',*,*,#2900,.T.);
#4011=ORIENTED_EDGE('',*,*,#2575,.T.);
#4012=ORIENTED_EDGE('',*,*,#2763,.F.);
#4013=ORIENTED_EDGE('',*,*,#2684,.F.);
#4014=ORIENTED_EDGE('',*,*,#2766,.F.);
#4015=ORIENTED_EDGE('',*,*,#2982,.T.);
#4016=ORIENTED_EDGE('',*,*,#2897,.T.);
#4017=ORIENTED_EDGE('',*,*,#2680,.F.);
#4018=ORIENTED_EDGE('',*,*,#2765,.F.);
#4019=ORIENTED_EDGE('',*,*,#2983,.F.);
#4020=ORIENTED_EDGE('',*,*,#2898,.F.);
#4021=ORIENTED_EDGE('',*,*,#2982,.F.);
#4022=ORIENTED_EDGE('',*,*,#2899,.T.);
#4023=ORIENTED_EDGE('',*,*,#2983,.T.);
#4024=ORIENTED_EDGE('',*,*,#2764,.F.);
#4025=ORIENTED_EDGE('',*,*,#2573,.T.);
#4026=ORIENTED_EDGE('',*,*,#2896,.T.);
#4027=ORIENTED_EDGE('',*,*,#2571,.T.);
#4028=ORIENTED_EDGE('',*,*,#2767,.F.);
#4029=ORIENTED_EDGE('',*,*,#2678,.F.);
#4030=ORIENTED_EDGE('',*,*,#2770,.F.);
#4031=ORIENTED_EDGE('',*,*,#2984,.T.);
#4032=ORIENTED_EDGE('',*,*,#2893,.T.);
#4033=ORIENTED_EDGE('',*,*,#2686,.F.);
#4034=ORIENTED_EDGE('',*,*,#2769,.F.);
#4035=ORIENTED_EDGE('',*,*,#2985,.F.);
#4036=ORIENTED_EDGE('',*,*,#2894,.F.);
#4037=ORIENTED_EDGE('',*,*,#2984,.F.);
#4038=ORIENTED_EDGE('',*,*,#2895,.T.);
#4039=ORIENTED_EDGE('',*,*,#2985,.T.);
#4040=ORIENTED_EDGE('',*,*,#2768,.F.);
#4041=ORIENTED_EDGE('',*,*,#2569,.T.);
#4042=ORIENTED_EDGE('',*,*,#2884,.T.);
#4043=ORIENTED_EDGE('',*,*,#2567,.T.);
#4044=ORIENTED_EDGE('',*,*,#2779,.F.);
#4045=ORIENTED_EDGE('',*,*,#2674,.F.);
#4046=ORIENTED_EDGE('',*,*,#2782,.F.);
#4047=ORIENTED_EDGE('',*,*,#2986,.T.);
#4048=ORIENTED_EDGE('',*,*,#2881,.T.);
#4049=ORIENTED_EDGE('',*,*,#2672,.F.);
#4050=ORIENTED_EDGE('',*,*,#2781,.F.);
#4051=ORIENTED_EDGE('',*,*,#2987,.F.);
#4052=ORIENTED_EDGE('',*,*,#2882,.F.);
#4053=ORIENTED_EDGE('',*,*,#2986,.F.);
#4054=ORIENTED_EDGE('',*,*,#2883,.T.);
#4055=ORIENTED_EDGE('',*,*,#2987,.T.);
#4056=ORIENTED_EDGE('',*,*,#2780,.F.);
#4057=ORIENTED_EDGE('',*,*,#2565,.T.);
#4058=ORIENTED_EDGE('',*,*,#2880,.T.);
#4059=ORIENTED_EDGE('',*,*,#2988,.T.);
#4060=ORIENTED_EDGE('',*,*,#2783,.F.);
#4061=ORIENTED_EDGE('',*,*,#2670,.F.);
#4062=ORIENTED_EDGE('',*,*,#2786,.F.);
#4063=ORIENTED_EDGE('',*,*,#2561,.T.);
#4064=ORIENTED_EDGE('',*,*,#2877,.T.);
#4065=ORIENTED_EDGE('',*,*,#2668,.F.);
#4066=ORIENTED_EDGE('',*,*,#2878,.T.);
#4067=ORIENTED_EDGE('',*,*,#2563,.T.);
#4068=ORIENTED_EDGE('',*,*,#2785,.F.);
#4069=ORIENTED_EDGE('',*,*,#2989,.T.);
#4070=ORIENTED_EDGE('',*,*,#2784,.F.);
#4071=ORIENTED_EDGE('',*,*,#2988,.F.);
#4072=ORIENTED_EDGE('',*,*,#2879,.F.);
#4073=ORIENTED_EDGE('',*,*,#2989,.F.);
#4074=ORIENTED_EDGE('',*,*,#2876,.T.);
#4075=ORIENTED_EDGE('',*,*,#2990,.T.);
#4076=ORIENTED_EDGE('',*,*,#2787,.F.);
#4077=ORIENTED_EDGE('',*,*,#2666,.F.);
#4078=ORIENTED_EDGE('',*,*,#2790,.F.);
#4079=ORIENTED_EDGE('',*,*,#2557,.T.);
#4080=ORIENTED_EDGE('',*,*,#2873,.T.);
#4081=ORIENTED_EDGE('',*,*,#2664,.F.);
#4082=ORIENTED_EDGE('',*,*,#2874,.T.);
#4083=ORIENTED_EDGE('',*,*,#2559,.T.);
#4084=ORIENTED_EDGE('',*,*,#2789,.F.);
#4085=ORIENTED_EDGE('',*,*,#2991,.T.);
#4086=ORIENTED_EDGE('',*,*,#2788,.F.);
#4087=ORIENTED_EDGE('',*,*,#2990,.F.);
#4088=ORIENTED_EDGE('',*,*,#2875,.F.);
#4089=ORIENTED_EDGE('',*,*,#2991,.F.);
#4090=ORIENTED_EDGE('',*,*,#2872,.T.);
#4091=ORIENTED_EDGE('',*,*,#2992,.T.);
#4092=ORIENTED_EDGE('',*,*,#2791,.F.);
#4093=ORIENTED_EDGE('',*,*,#2662,.F.);
#4094=ORIENTED_EDGE('',*,*,#2794,.F.);
#4095=ORIENTED_EDGE('',*,*,#2553,.T.);
#4096=ORIENTED_EDGE('',*,*,#2869,.T.);
#4097=ORIENTED_EDGE('',*,*,#2656,.F.);
#4098=ORIENTED_EDGE('',*,*,#2870,.T.);
#4099=ORIENTED_EDGE('',*,*,#2555,.T.);
#4100=ORIENTED_EDGE('',*,*,#2793,.F.);
#4101=ORIENTED_EDGE('',*,*,#2993,.T.);
#4102=ORIENTED_EDGE('',*,*,#2792,.F.);
#4103=ORIENTED_EDGE('',*,*,#2992,.F.);
#4104=ORIENTED_EDGE('',*,*,#2871,.F.);
#4105=ORIENTED_EDGE('',*,*,#2993,.F.);
#4106=ORIENTED_EDGE('',*,*,#2864,.T.);
#4107=ORIENTED_EDGE('',*,*,#2994,.T.);
#4108=ORIENTED_EDGE('',*,*,#2799,.F.);
#4109=ORIENTED_EDGE('',*,*,#2660,.F.);
#4110=ORIENTED_EDGE('',*,*,#2802,.F.);
#4111=ORIENTED_EDGE('',*,*,#2549,.T.);
#4112=ORIENTED_EDGE('',*,*,#2861,.T.);
#4113=ORIENTED_EDGE('',*,*,#2652,.F.);
#4114=ORIENTED_EDGE('',*,*,#2862,.T.);
#4115=ORIENTED_EDGE('',*,*,#2551,.T.);
#4116=ORIENTED_EDGE('',*,*,#2801,.F.);
#4117=ORIENTED_EDGE('',*,*,#2995,.T.);
#4118=ORIENTED_EDGE('',*,*,#2800,.F.);
#4119=ORIENTED_EDGE('',*,*,#2994,.F.);
#4120=ORIENTED_EDGE('',*,*,#2863,.F.);
#4121=ORIENTED_EDGE('',*,*,#2995,.F.);
#4122=ORIENTED_EDGE('',*,*,#2868,.T.);
#4123=ORIENTED_EDGE('',*,*,#2996,.T.);
#4124=ORIENTED_EDGE('',*,*,#2795,.F.);
#4125=ORIENTED_EDGE('',*,*,#2654,.F.);
#4126=ORIENTED_EDGE('',*,*,#2798,.F.);
#4127=ORIENTED_EDGE('',*,*,#2545,.T.);
#4128=ORIENTED_EDGE('',*,*,#2865,.T.);
#4129=ORIENTED_EDGE('',*,*,#2658,.F.);
#4130=ORIENTED_EDGE('',*,*,#2866,.T.);
#4131=ORIENTED_EDGE('',*,*,#2547,.T.);
#4132=ORIENTED_EDGE('',*,*,#2797,.F.);
#4133=ORIENTED_EDGE('',*,*,#2997,.T.);
#4134=ORIENTED_EDGE('',*,*,#2796,.F.);
#4135=ORIENTED_EDGE('',*,*,#2996,.F.);
#4136=ORIENTED_EDGE('',*,*,#2867,.F.);
#4137=ORIENTED_EDGE('',*,*,#2997,.F.);
#4138=ORIENTED_EDGE('',*,*,#2860,.T.);
#4139=ORIENTED_EDGE('',*,*,#2998,.T.);
#4140=ORIENTED_EDGE('',*,*,#2803,.F.);
#4141=ORIENTED_EDGE('',*,*,#2650,.F.);
#4142=ORIENTED_EDGE('',*,*,#2858,.T.);
#4143=ORIENTED_EDGE('',*,*,#2540,.T.);
#4144=ORIENTED_EDGE('',*,*,#2805,.F.);
#4145=ORIENTED_EDGE('',*,*,#2999,.T.);
#4146=ORIENTED_EDGE('',*,*,#2804,.F.);
#4147=ORIENTED_EDGE('',*,*,#2998,.F.);
#4148=ORIENTED_EDGE('',*,*,#2859,.F.);
#4149=ORIENTED_EDGE('',*,*,#2999,.F.);
#4150=ORIENTED_EDGE('',*,*,#2857,.T.);
#4151=ORIENTED_EDGE('',*,*,#3000,.T.);
#4152=ORIENTED_EDGE('',*,*,#2806,.F.);
#4153=ORIENTED_EDGE('',*,*,#2647,.F.);
#4154=ORIENTED_EDGE('',*,*,#2855,.T.);
#4155=ORIENTED_EDGE('',*,*,#2533,.T.);
#4156=ORIENTED_EDGE('',*,*,#2808,.F.);
#4157=ORIENTED_EDGE('',*,*,#3001,.T.);
#4158=ORIENTED_EDGE('',*,*,#2807,.F.);
#4159=ORIENTED_EDGE('',*,*,#3000,.F.);
#4160=ORIENTED_EDGE('',*,*,#2856,.F.);
#4161=ORIENTED_EDGE('',*,*,#3001,.F.);
#4162=ORIENTED_EDGE('',*,*,#2762,.F.);
#4163=ORIENTED_EDGE('',*,*,#3002,.T.);
#4164=ORIENTED_EDGE('',*,*,#2901,.T.);
#4165=ORIENTED_EDGE('',*,*,#2682,.F.);
#4166=ORIENTED_EDGE('',*,*,#2761,.F.);
#4167=ORIENTED_EDGE('',*,*,#3003,.F.);
#4168=ORIENTED_EDGE('',*,*,#2902,.F.);
#4169=ORIENTED_EDGE('',*,*,#3002,.F.);
#4170=ORIENTED_EDGE('',*,*,#2903,.T.);
#4171=ORIENTED_EDGE('',*,*,#3003,.T.);
#4172=ORIENTED_EDGE('',*,*,#2760,.F.);
#4173=ORIENTED_EDGE('',*,*,#2524,.T.);
#4174=ORIENTED_EDGE('',*,*,#2759,.F.);
#4175=ORIENTED_EDGE('',*,*,#3004,.T.);
#4176=ORIENTED_EDGE('',*,*,#2904,.T.);
#4177=ORIENTED_EDGE('',*,*,#2644,.F.);
#4178=ORIENTED_EDGE('',*,*,#2758,.F.);
#4179=ORIENTED_EDGE('',*,*,#3005,.F.);
#4180=ORIENTED_EDGE('',*,*,#2905,.F.);
#4181=ORIENTED_EDGE('',*,*,#3004,.F.);
#4182=ORIENTED_EDGE('',*,*,#2906,.T.);
#4183=ORIENTED_EDGE('',*,*,#3005,.T.);
#4184=ORIENTED_EDGE('',*,*,#2757,.F.);
#4185=ORIENTED_EDGE('',*,*,#2517,.T.);
#4186=ORIENTED_EDGE('',*,*,#2911,.T.);
#4187=ORIENTED_EDGE('',*,*,#3006,.T.);
#4188=ORIENTED_EDGE('',*,*,#2752,.F.);
#4189=ORIENTED_EDGE('',*,*,#2639,.F.);
#4190=ORIENTED_EDGE('',*,*,#2756,.F.);
#4191=ORIENTED_EDGE('',*,*,#3007,.T.);
#4192=ORIENTED_EDGE('',*,*,#2907,.T.);
#4193=ORIENTED_EDGE('',*,*,#2641,.F.);
#4194=ORIENTED_EDGE('',*,*,#2755,.F.);
#4195=ORIENTED_EDGE('',*,*,#3008,.F.);
#4196=ORIENTED_EDGE('',*,*,#2908,.F.);
#4197=ORIENTED_EDGE('',*,*,#3007,.F.);
#4198=ORIENTED_EDGE('',*,*,#2909,.T.);
#4199=ORIENTED_EDGE('',*,*,#3008,.T.);
#4200=ORIENTED_EDGE('',*,*,#2754,.F.);
#4201=ORIENTED_EDGE('',*,*,#3009,.T.);
#4202=ORIENTED_EDGE('',*,*,#2753,.F.);
#4203=ORIENTED_EDGE('',*,*,#3006,.F.);
#4204=ORIENTED_EDGE('',*,*,#2910,.F.);
#4205=ORIENTED_EDGE('',*,*,#3009,.F.);
#4206=ORIENTED_EDGE('',*,*,#2916,.T.);
#4207=ORIENTED_EDGE('',*,*,#3010,.T.);
#4208=ORIENTED_EDGE('',*,*,#2747,.F.);
#4209=ORIENTED_EDGE('',*,*,#2635,.F.);
#4210=ORIENTED_EDGE('',*,*,#2751,.F.);
#4211=ORIENTED_EDGE('',*,*,#3011,.T.);
#4212=ORIENTED_EDGE('',*,*,#2912,.T.);
#4213=ORIENTED_EDGE('',*,*,#2637,.F.);
#4214=ORIENTED_EDGE('',*,*,#2750,.F.);
#4215=ORIENTED_EDGE('',*,*,#3012,.F.);
#4216=ORIENTED_EDGE('',*,*,#2913,.F.);
#4217=ORIENTED_EDGE('',*,*,#3011,.F.);
#4218=ORIENTED_EDGE('',*,*,#2914,.T.);
#4219=ORIENTED_EDGE('',*,*,#3012,.T.);
#4220=ORIENTED_EDGE('',*,*,#2749,.F.);
#4221=ORIENTED_EDGE('',*,*,#3013,.T.);
#4222=ORIENTED_EDGE('',*,*,#2748,.F.);
#4223=ORIENTED_EDGE('',*,*,#3010,.F.);
#4224=ORIENTED_EDGE('',*,*,#2915,.F.);
#4225=ORIENTED_EDGE('',*,*,#3013,.F.);
#4226=ORIENTED_EDGE('',*,*,#2931,.T.);
#4227=ORIENTED_EDGE('',*,*,#3014,.T.);
#4228=ORIENTED_EDGE('',*,*,#2732,.F.);
#4229=ORIENTED_EDGE('',*,*,#2631,.F.);
#4230=ORIENTED_EDGE('',*,*,#2736,.F.);
#4231=ORIENTED_EDGE('',*,*,#3015,.T.);
#4232=ORIENTED_EDGE('',*,*,#2927,.T.);
#4233=ORIENTED_EDGE('',*,*,#2623,.F.);
#4234=ORIENTED_EDGE('',*,*,#2735,.F.);
#4235=ORIENTED_EDGE('',*,*,#3016,.F.);
#4236=ORIENTED_EDGE('',*,*,#2928,.F.);
#4237=ORIENTED_EDGE('',*,*,#3015,.F.);
#4238=ORIENTED_EDGE('',*,*,#2929,.T.);
#4239=ORIENTED_EDGE('',*,*,#3016,.T.);
#4240=ORIENTED_EDGE('',*,*,#2734,.F.);
#4241=ORIENTED_EDGE('',*,*,#3017,.T.);
#4242=ORIENTED_EDGE('',*,*,#2733,.F.);
#4243=ORIENTED_EDGE('',*,*,#3014,.F.);
#4244=ORIENTED_EDGE('',*,*,#2930,.F.);
#4245=ORIENTED_EDGE('',*,*,#3017,.F.);
#4246=ORIENTED_EDGE('',*,*,#2936,.T.);
#4247=ORIENTED_EDGE('',*,*,#3018,.T.);
#4248=ORIENTED_EDGE('',*,*,#2727,.F.);
#4249=ORIENTED_EDGE('',*,*,#2627,.F.);
#4250=ORIENTED_EDGE('',*,*,#2731,.F.);
#4251=ORIENTED_EDGE('',*,*,#3019,.T.);
#4252=ORIENTED_EDGE('',*,*,#2932,.T.);
#4253=ORIENTED_EDGE('',*,*,#2629,.F.);
#4254=ORIENTED_EDGE('',*,*,#2730,.F.);
#4255=ORIENTED_EDGE('',*,*,#3020,.F.);
#4256=ORIENTED_EDGE('',*,*,#2933,.F.);
#4257=ORIENTED_EDGE('',*,*,#3019,.F.);
#4258=ORIENTED_EDGE('',*,*,#2934,.T.);
#4259=ORIENTED_EDGE('',*,*,#3020,.T.);
#4260=ORIENTED_EDGE('',*,*,#2729,.F.);
#4261=ORIENTED_EDGE('',*,*,#3021,.T.);
#4262=ORIENTED_EDGE('',*,*,#2728,.F.);
#4263=ORIENTED_EDGE('',*,*,#3018,.F.);
#4264=ORIENTED_EDGE('',*,*,#2935,.F.);
#4265=ORIENTED_EDGE('',*,*,#3021,.F.);
#4266=ORIENTED_EDGE('',*,*,#2926,.T.);
#4267=ORIENTED_EDGE('',*,*,#3022,.T.);
#4268=ORIENTED_EDGE('',*,*,#2737,.F.);
#4269=ORIENTED_EDGE('',*,*,#2621,.F.);
#4270=ORIENTED_EDGE('',*,*,#2741,.F.);
#4271=ORIENTED_EDGE('',*,*,#3023,.T.);
#4272=ORIENTED_EDGE('',*,*,#2922,.T.);
#4273=ORIENTED_EDGE('',*,*,#2619,.F.);
#4274=ORIENTED_EDGE('',*,*,#2740,.F.);
#4275=ORIENTED_EDGE('',*,*,#3024,.F.);
#4276=ORIENTED_EDGE('',*,*,#2923,.F.);
#4277=ORIENTED_EDGE('',*,*,#3023,.F.);
#4278=ORIENTED_EDGE('',*,*,#2924,.T.);
#4279=ORIENTED_EDGE('',*,*,#3024,.T.);
#4280=ORIENTED_EDGE('',*,*,#2739,.F.);
#4281=ORIENTED_EDGE('',*,*,#3025,.T.);
#4282=ORIENTED_EDGE('',*,*,#2738,.F.);
#4283=ORIENTED_EDGE('',*,*,#3022,.F.);
#4284=ORIENTED_EDGE('',*,*,#2925,.F.);
#4285=ORIENTED_EDGE('',*,*,#3025,.F.);
#4286=ORIENTED_EDGE('',*,*,#2921,.T.);
#4287=ORIENTED_EDGE('',*,*,#3026,.T.);
#4288=ORIENTED_EDGE('',*,*,#2742,.F.);
#4289=ORIENTED_EDGE('',*,*,#2617,.F.);
#4290=ORIENTED_EDGE('',*,*,#2746,.F.);
#4291=ORIENTED_EDGE('',*,*,#3027,.T.);
#4292=ORIENTED_EDGE('',*,*,#2917,.T.);
#4293=ORIENTED_EDGE('',*,*,#2633,.F.);
#4294=ORIENTED_EDGE('',*,*,#2745,.F.);
#4295=ORIENTED_EDGE('',*,*,#3028,.F.);
#4296=ORIENTED_EDGE('',*,*,#2918,.F.);
#4297=ORIENTED_EDGE('',*,*,#3027,.F.);
#4298=ORIENTED_EDGE('',*,*,#2919,.T.);
#4299=ORIENTED_EDGE('',*,*,#3028,.T.);
#4300=ORIENTED_EDGE('',*,*,#2744,.F.);
#4301=ORIENTED_EDGE('',*,*,#3029,.T.);
#4302=ORIENTED_EDGE('',*,*,#2743,.F.);
#4303=ORIENTED_EDGE('',*,*,#3026,.F.);
#4304=ORIENTED_EDGE('',*,*,#2920,.F.);
#4305=ORIENTED_EDGE('',*,*,#3029,.F.);
#4306=ORIENTED_EDGE('',*,*,#2941,.T.);
#4307=ORIENTED_EDGE('',*,*,#3030,.T.);
#4308=ORIENTED_EDGE('',*,*,#2722,.F.);
#4309=ORIENTED_EDGE('',*,*,#2615,.F.);
#4310=ORIENTED_EDGE('',*,*,#2726,.F.);
#4311=ORIENTED_EDGE('',*,*,#3031,.T.);
#4312=ORIENTED_EDGE('',*,*,#2937,.T.);
#4313=ORIENTED_EDGE('',*,*,#2625,.F.);
#4314=ORIENTED_EDGE('',*,*,#2725,.F.);
#4315=ORIENTED_EDGE('',*,*,#3032,.F.);
#4316=ORIENTED_EDGE('',*,*,#2938,.F.);
#4317=ORIENTED_EDGE('',*,*,#3031,.F.);
#4318=ORIENTED_EDGE('',*,*,#2939,.T.);
#4319=ORIENTED_EDGE('',*,*,#3032,.T.);
#4320=ORIENTED_EDGE('',*,*,#2724,.F.);
#4321=ORIENTED_EDGE('',*,*,#3033,.T.);
#4322=ORIENTED_EDGE('',*,*,#2723,.F.);
#4323=ORIENTED_EDGE('',*,*,#3030,.F.);
#4324=ORIENTED_EDGE('',*,*,#2940,.F.);
#4325=ORIENTED_EDGE('',*,*,#3033,.F.);
#4326=ORIENTED_EDGE('',*,*,#2946,.T.);
#4327=ORIENTED_EDGE('',*,*,#3034,.T.);
#4328=ORIENTED_EDGE('',*,*,#2717,.F.);
#4329=ORIENTED_EDGE('',*,*,#2585,.F.);
#4330=ORIENTED_EDGE('',*,*,#2721,.F.);
#4331=ORIENTED_EDGE('',*,*,#3035,.T.);
#4332=ORIENTED_EDGE('',*,*,#2942,.T.);
#4333=ORIENTED_EDGE('',*,*,#2613,.F.);
#4334=ORIENTED_EDGE('',*,*,#2720,.F.);
#4335=ORIENTED_EDGE('',*,*,#3036,.F.);
#4336=ORIENTED_EDGE('',*,*,#2943,.F.);
#4337=ORIENTED_EDGE('',*,*,#3035,.F.);
#4338=ORIENTED_EDGE('',*,*,#2944,.T.);
#4339=ORIENTED_EDGE('',*,*,#3036,.T.);
#4340=ORIENTED_EDGE('',*,*,#2719,.F.);
#4341=ORIENTED_EDGE('',*,*,#3037,.T.);
#4342=ORIENTED_EDGE('',*,*,#2718,.F.);
#4343=ORIENTED_EDGE('',*,*,#3034,.F.);
#4344=ORIENTED_EDGE('',*,*,#2945,.F.);
#4345=ORIENTED_EDGE('',*,*,#3037,.F.);
#4346=ORIENTED_EDGE('',*,*,#2951,.T.);
#4347=ORIENTED_EDGE('',*,*,#3038,.T.);
#4348=ORIENTED_EDGE('',*,*,#2712,.F.);
#4349=ORIENTED_EDGE('',*,*,#2611,.F.);
#4350=ORIENTED_EDGE('',*,*,#2716,.F.);
#4351=ORIENTED_EDGE('',*,*,#3039,.T.);
#4352=ORIENTED_EDGE('',*,*,#2947,.T.);
#4353=ORIENTED_EDGE('',*,*,#2587,.F.);
#4354=ORIENTED_EDGE('',*,*,#2715,.F.);
#4355=ORIENTED_EDGE('',*,*,#3040,.F.);
#4356=ORIENTED_EDGE('',*,*,#2948,.F.);
#4357=ORIENTED_EDGE('',*,*,#3039,.F.);
#4358=ORIENTED_EDGE('',*,*,#2949,.T.);
#4359=ORIENTED_EDGE('',*,*,#3040,.T.);
#4360=ORIENTED_EDGE('',*,*,#2714,.F.);
#4361=ORIENTED_EDGE('',*,*,#3041,.T.);
#4362=ORIENTED_EDGE('',*,*,#2713,.F.);
#4363=ORIENTED_EDGE('',*,*,#3038,.F.);
#4364=ORIENTED_EDGE('',*,*,#2950,.F.);
#4365=ORIENTED_EDGE('',*,*,#3041,.F.);
#4366=ORIENTED_EDGE('',*,*,#2956,.T.);
#4367=ORIENTED_EDGE('',*,*,#3042,.T.);
#4368=ORIENTED_EDGE('',*,*,#2707,.F.);
#4369=ORIENTED_EDGE('',*,*,#2607,.F.);
#4370=ORIENTED_EDGE('',*,*,#2711,.F.);
#4371=ORIENTED_EDGE('',*,*,#3043,.T.);
#4372=ORIENTED_EDGE('',*,*,#2952,.T.);
#4373=ORIENTED_EDGE('',*,*,#2609,.F.);
#4374=ORIENTED_EDGE('',*,*,#2710,.F.);
#4375=ORIENTED_EDGE('',*,*,#3044,.F.);
#4376=ORIENTED_EDGE('',*,*,#2953,.F.);
#4377=ORIENTED_EDGE('',*,*,#3043,.F.);
#4378=ORIENTED_EDGE('',*,*,#2954,.T.);
#4379=ORIENTED_EDGE('',*,*,#3044,.T.);
#4380=ORIENTED_EDGE('',*,*,#2709,.F.);
#4381=ORIENTED_EDGE('',*,*,#3045,.T.);
#4382=ORIENTED_EDGE('',*,*,#2708,.F.);
#4383=ORIENTED_EDGE('',*,*,#3042,.F.);
#4384=ORIENTED_EDGE('',*,*,#2955,.F.);
#4385=ORIENTED_EDGE('',*,*,#3045,.F.);
#4386=ORIENTED_EDGE('',*,*,#2843,.T.);
#4387=ORIENTED_EDGE('',*,*,#3046,.T.);
#4388=ORIENTED_EDGE('',*,*,#2820,.F.);
#4389=ORIENTED_EDGE('',*,*,#2601,.F.);
#4390=ORIENTED_EDGE('',*,*,#2824,.F.);
#4391=ORIENTED_EDGE('',*,*,#3047,.T.);
#4392=ORIENTED_EDGE('',*,*,#2839,.T.);
#4393=ORIENTED_EDGE('',*,*,#2599,.F.);
#4394=ORIENTED_EDGE('',*,*,#2823,.F.);
#4395=ORIENTED_EDGE('',*,*,#3048,.F.);
#4396=ORIENTED_EDGE('',*,*,#2840,.F.);
#4397=ORIENTED_EDGE('',*,*,#3047,.F.);
#4398=ORIENTED_EDGE('',*,*,#2841,.T.);
#4399=ORIENTED_EDGE('',*,*,#3048,.T.);
#4400=ORIENTED_EDGE('',*,*,#2822,.F.);
#4401=ORIENTED_EDGE('',*,*,#3049,.T.);
#4402=ORIENTED_EDGE('',*,*,#2821,.F.);
#4403=ORIENTED_EDGE('',*,*,#3046,.F.);
#4404=ORIENTED_EDGE('',*,*,#2842,.F.);
#4405=ORIENTED_EDGE('',*,*,#3049,.F.);
#4406=ORIENTED_EDGE('',*,*,#2838,.T.);
#4407=ORIENTED_EDGE('',*,*,#3050,.T.);
#4408=ORIENTED_EDGE('',*,*,#2825,.F.);
#4409=ORIENTED_EDGE('',*,*,#2597,.F.);
#4410=ORIENTED_EDGE('',*,*,#2829,.F.);
#4411=ORIENTED_EDGE('',*,*,#3051,.T.);
#4412=ORIENTED_EDGE('',*,*,#2834,.T.);
#4413=ORIENTED_EDGE('',*,*,#2591,.F.);
#4414=ORIENTED_EDGE('',*,*,#2828,.F.);
#4415=ORIENTED_EDGE('',*,*,#3052,.F.);
#4416=ORIENTED_EDGE('',*,*,#2835,.F.);
#4417=ORIENTED_EDGE('',*,*,#3051,.F.);
#4418=ORIENTED_EDGE('',*,*,#2836,.T.);
#4419=ORIENTED_EDGE('',*,*,#3052,.T.);
#4420=ORIENTED_EDGE('',*,*,#2827,.F.);
#4421=ORIENTED_EDGE('',*,*,#3053,.T.);
#4422=ORIENTED_EDGE('',*,*,#2826,.F.);
#4423=ORIENTED_EDGE('',*,*,#3050,.F.);
#4424=ORIENTED_EDGE('',*,*,#2837,.F.);
#4425=ORIENTED_EDGE('',*,*,#3053,.F.);
#4426=ORIENTED_EDGE('',*,*,#2961,.T.);
#4427=ORIENTED_EDGE('',*,*,#3054,.T.);
#4428=ORIENTED_EDGE('',*,*,#2702,.F.);
#4429=ORIENTED_EDGE('',*,*,#2595,.F.);
#4430=ORIENTED_EDGE('',*,*,#2706,.F.);
#4431=ORIENTED_EDGE('',*,*,#3055,.T.);
#4432=ORIENTED_EDGE('',*,*,#2957,.T.);
#4433=ORIENTED_EDGE('',*,*,#2605,.F.);
#4434=ORIENTED_EDGE('',*,*,#2705,.F.);
#4435=ORIENTED_EDGE('',*,*,#3056,.F.);
#4436=ORIENTED_EDGE('',*,*,#2958,.F.);
#4437=ORIENTED_EDGE('',*,*,#3055,.F.);
#4438=ORIENTED_EDGE('',*,*,#2959,.T.);
#4439=ORIENTED_EDGE('',*,*,#3056,.T.);
#4440=ORIENTED_EDGE('',*,*,#2704,.F.);
#4441=ORIENTED_EDGE('',*,*,#3057,.T.);
#4442=ORIENTED_EDGE('',*,*,#2703,.F.);
#4443=ORIENTED_EDGE('',*,*,#3054,.F.);
#4444=ORIENTED_EDGE('',*,*,#2960,.F.);
#4445=ORIENTED_EDGE('',*,*,#3057,.F.);
#4446=ORIENTED_EDGE('',*,*,#2833,.T.);
#4447=ORIENTED_EDGE('',*,*,#3058,.T.);
#4448=ORIENTED_EDGE('',*,*,#2697,.F.);
#4449=ORIENTED_EDGE('',*,*,#2589,.F.);
#4450=ORIENTED_EDGE('',*,*,#2701,.F.);
#4451=ORIENTED_EDGE('',*,*,#3059,.T.);
#4452=ORIENTED_EDGE('',*,*,#2962,.T.);
#4453=ORIENTED_EDGE('',*,*,#2593,.F.);
#4454=ORIENTED_EDGE('',*,*,#2700,.F.);
#4455=ORIENTED_EDGE('',*,*,#3060,.F.);
#4456=ORIENTED_EDGE('',*,*,#2963,.F.);
#4457=ORIENTED_EDGE('',*,*,#3059,.F.);
#4458=ORIENTED_EDGE('',*,*,#2964,.T.);
#4459=ORIENTED_EDGE('',*,*,#3060,.T.);
#4460=ORIENTED_EDGE('',*,*,#2699,.F.);
#4461=ORIENTED_EDGE('',*,*,#3061,.T.);
#4462=ORIENTED_EDGE('',*,*,#2698,.F.);
#4463=ORIENTED_EDGE('',*,*,#3058,.F.);
#4464=ORIENTED_EDGE('',*,*,#2965,.F.);
#4465=ORIENTED_EDGE('',*,*,#3061,.F.);
#4466=ORIENTED_EDGE('',*,*,#3062,.T.);
#4467=ORIENTED_EDGE('',*,*,#2967,.T.);
#4468=ORIENTED_EDGE('',*,*,#3063,.F.);
#4469=ORIENTED_EDGE('',*,*,#2830,.F.);
#4470=ORIENTED_EDGE('',*,*,#3063,.T.);
#4471=ORIENTED_EDGE('',*,*,#2966,.T.);
#4472=ORIENTED_EDGE('',*,*,#2513,.F.);
#4473=ORIENTED_EDGE('',*,*,#2831,.F.);
#4474=ORIENTED_EDGE('',*,*,#2515,.F.);
#4475=ORIENTED_EDGE('',*,*,#2968,.T.);
#4476=ORIENTED_EDGE('',*,*,#3062,.F.);
#4477=ORIENTED_EDGE('',*,*,#2832,.F.);
#4478=ORIENTED_EDGE('',*,*,#3064,.F.);
#4479=ORIENTED_EDGE('',*,*,#3065,.T.);
#4480=ORIENTED_EDGE('',*,*,#3066,.T.);
#4481=ORIENTED_EDGE('',*,*,#3065,.F.);
#4482=ORIENTED_EDGE('',*,*,#3067,.T.);
#4483=ORIENTED_EDGE('',*,*,#3068,.F.);
#4484=ORIENTED_EDGE('',*,*,#3069,.F.);
#4485=ORIENTED_EDGE('',*,*,#3070,.T.);
#4486=ORIENTED_EDGE('',*,*,#3071,.T.);
#4487=ORIENTED_EDGE('',*,*,#3072,.T.);
#4488=ORIENTED_EDGE('',*,*,#3073,.F.);
#4489=ORIENTED_EDGE('',*,*,#3068,.T.);
#4490=ORIENTED_EDGE('',*,*,#3074,.T.);
#4491=ORIENTED_EDGE('',*,*,#3075,.T.);
#4492=ORIENTED_EDGE('',*,*,#3076,.F.);
#4493=ORIENTED_EDGE('',*,*,#3072,.F.);
#4494=ORIENTED_EDGE('',*,*,#3077,.F.);
#4495=ORIENTED_EDGE('',*,*,#3078,.T.);
#4496=ORIENTED_EDGE('',*,*,#3069,.T.);
#4497=ORIENTED_EDGE('',*,*,#3073,.T.);
#4498=ORIENTED_EDGE('',*,*,#3071,.F.);
#4499=ORIENTED_EDGE('',*,*,#3079,.F.);
#4500=ORIENTED_EDGE('',*,*,#3080,.F.);
#4501=ORIENTED_EDGE('',*,*,#3081,.T.);
#4502=ORIENTED_EDGE('',*,*,#3082,.T.);
#4503=ORIENTED_EDGE('',*,*,#3077,.T.);
#4504=ORIENTED_EDGE('',*,*,#3083,.F.);
#4505=ORIENTED_EDGE('',*,*,#3084,.F.);
#4506=ORIENTED_EDGE('',*,*,#3085,.F.);
#4507=ORIENTED_EDGE('',*,*,#3086,.T.);
#4508=ORIENTED_EDGE('',*,*,#3087,.T.);
#4509=ORIENTED_EDGE('',*,*,#3080,.T.);
#4510=ORIENTED_EDGE('',*,*,#3088,.F.);
#4511=ORIENTED_EDGE('',*,*,#3089,.F.);
#4512=ORIENTED_EDGE('',*,*,#3090,.F.);
#4513=ORIENTED_EDGE('',*,*,#3091,.T.);
#4514=ORIENTED_EDGE('',*,*,#3092,.T.);
#4515=ORIENTED_EDGE('',*,*,#3085,.T.);
#4516=ORIENTED_EDGE('',*,*,#3093,.F.);
#4517=ORIENTED_EDGE('',*,*,#3094,.F.);
#4518=ORIENTED_EDGE('',*,*,#3075,.F.);
#4519=ORIENTED_EDGE('',*,*,#3095,.T.);
#4520=ORIENTED_EDGE('',*,*,#3096,.T.);
#4521=ORIENTED_EDGE('',*,*,#3090,.T.);
#4522=ORIENTED_EDGE('',*,*,#3097,.F.);
#4523=ORIENTED_EDGE('',*,*,#3098,.F.);
#4524=ORIENTED_EDGE('',*,*,#3089,.T.);
#4525=ORIENTED_EDGE('',*,*,#3099,.T.);
#4526=ORIENTED_EDGE('',*,*,#3093,.T.);
#4527=ORIENTED_EDGE('',*,*,#3084,.T.);
#4528=ORIENTED_EDGE('',*,*,#3100,.T.);
#4529=ORIENTED_EDGE('',*,*,#3088,.T.);
#4530=ORIENTED_EDGE('',*,*,#3083,.T.);
#4531=ORIENTED_EDGE('',*,*,#3079,.T.);
#4532=ORIENTED_EDGE('',*,*,#3101,.T.);
#4533=ORIENTED_EDGE('',*,*,#3076,.T.);
#4534=ORIENTED_EDGE('',*,*,#3098,.T.);
#4535=ORIENTED_EDGE('',*,*,#3102,.F.);
#4536=ORIENTED_EDGE('',*,*,#3094,.T.);
#4537=ORIENTED_EDGE('',*,*,#3103,.T.);
#4538=ORIENTED_EDGE('',*,*,#3097,.T.);
#4539=ORIENTED_EDGE('',*,*,#3103,.F.);
#4540=ORIENTED_EDGE('',*,*,#3099,.F.);
#4541=ORIENTED_EDGE('',*,*,#3100,.F.);
#4542=ORIENTED_EDGE('',*,*,#3101,.F.);
#4543=ORIENTED_EDGE('',*,*,#3070,.F.);
#4544=ORIENTED_EDGE('',*,*,#3102,.T.);
#4545=ORIENTED_EDGE('',*,*,#3066,.F.);
#4546=ORIENTED_EDGE('',*,*,#3092,.F.);
#4547=ORIENTED_EDGE('',*,*,#3104,.T.);
#4548=ORIENTED_EDGE('',*,*,#3086,.F.);
#4549=ORIENTED_EDGE('',*,*,#3096,.F.);
#4550=ORIENTED_EDGE('',*,*,#3105,.T.);
#4551=ORIENTED_EDGE('',*,*,#3091,.F.);
#4552=ORIENTED_EDGE('',*,*,#3106,.T.);
#4553=ORIENTED_EDGE('',*,*,#3095,.F.);
#4554=ORIENTED_EDGE('',*,*,#3074,.F.);
#4555=ORIENTED_EDGE('',*,*,#3107,.T.);
#4556=ORIENTED_EDGE('',*,*,#3078,.F.);
#4557=ORIENTED_EDGE('',*,*,#3082,.F.);
#4558=ORIENTED_EDGE('',*,*,#3087,.F.);
#4559=ORIENTED_EDGE('',*,*,#3108,.T.);
#4560=ORIENTED_EDGE('',*,*,#3081,.F.);
#4561=ORIENTED_EDGE('',*,*,#3108,.F.);
#4562=ORIENTED_EDGE('',*,*,#3104,.F.);
#4563=ORIENTED_EDGE('',*,*,#3105,.F.);
#4564=ORIENTED_EDGE('',*,*,#3106,.F.);
#4565=ORIENTED_EDGE('',*,*,#3067,.F.);
#4566=ORIENTED_EDGE('',*,*,#3107,.F.);
#4567=ORIENTED_EDGE('',*,*,#3064,.T.);
#4568=ORIENTED_EDGE('',*,*,#3109,.T.);
#4569=ORIENTED_EDGE('',*,*,#3110,.T.);
#4570=ORIENTED_EDGE('',*,*,#3111,.F.);
#4571=ORIENTED_EDGE('',*,*,#3110,.F.);
#4572=ORIENTED_EDGE('',*,*,#3112,.T.);
#4573=ORIENTED_EDGE('',*,*,#3113,.T.);
#4574=ORIENTED_EDGE('',*,*,#3114,.F.);
#4575=ORIENTED_EDGE('',*,*,#3113,.F.);
#4576=ORIENTED_EDGE('',*,*,#3115,.T.);
#4577=ORIENTED_EDGE('',*,*,#3116,.T.);
#4578=ORIENTED_EDGE('',*,*,#3117,.F.);
#4579=ORIENTED_EDGE('',*,*,#3116,.F.);
#4580=ORIENTED_EDGE('',*,*,#3118,.T.);
#4581=ORIENTED_EDGE('',*,*,#3119,.T.);
#4582=ORIENTED_EDGE('',*,*,#3120,.F.);
#4583=ORIENTED_EDGE('',*,*,#3119,.F.);
#4584=ORIENTED_EDGE('',*,*,#3121,.T.);
#4585=ORIENTED_EDGE('',*,*,#3122,.T.);
#4586=ORIENTED_EDGE('',*,*,#3123,.F.);
#4587=ORIENTED_EDGE('',*,*,#3122,.F.);
#4588=ORIENTED_EDGE('',*,*,#3124,.T.);
#4589=ORIENTED_EDGE('',*,*,#3125,.T.);
#4590=ORIENTED_EDGE('',*,*,#3126,.F.);
#4591=ORIENTED_EDGE('',*,*,#3125,.F.);
#4592=ORIENTED_EDGE('',*,*,#3127,.T.);
#4593=ORIENTED_EDGE('',*,*,#3128,.T.);
#4594=ORIENTED_EDGE('',*,*,#3129,.F.);
#4595=ORIENTED_EDGE('',*,*,#3128,.F.);
#4596=ORIENTED_EDGE('',*,*,#3114,.T.);
#4597=ORIENTED_EDGE('',*,*,#3115,.F.);
#4598=ORIENTED_EDGE('',*,*,#3118,.F.);
#4599=ORIENTED_EDGE('',*,*,#3121,.F.);
#4600=ORIENTED_EDGE('',*,*,#3124,.F.);
#4601=ORIENTED_EDGE('',*,*,#3127,.F.);
#4602=ORIENTED_EDGE('',*,*,#3112,.F.);
#4603=ORIENTED_EDGE('',*,*,#3111,.T.);
#4604=ORIENTED_EDGE('',*,*,#3117,.T.);
#4605=ORIENTED_EDGE('',*,*,#3120,.T.);
#4606=ORIENTED_EDGE('',*,*,#3123,.T.);
#4607=ORIENTED_EDGE('',*,*,#3126,.T.);
#4608=ORIENTED_EDGE('',*,*,#3129,.T.);
#4609=ORIENTED_EDGE('',*,*,#3109,.F.);
#4610=ORIENTED_EDGE('',*,*,#3130,.T.);
#4611=ORIENTED_EDGE('',*,*,#3131,.T.);
#4612=ORIENTED_EDGE('',*,*,#3132,.F.);
#4613=ORIENTED_EDGE('',*,*,#3131,.F.);
#4614=ORIENTED_EDGE('',*,*,#3133,.T.);
#4615=ORIENTED_EDGE('',*,*,#3134,.T.);
#4616=ORIENTED_EDGE('',*,*,#3135,.F.);
#4617=ORIENTED_EDGE('',*,*,#3134,.F.);
#4618=ORIENTED_EDGE('',*,*,#3135,.T.);
#4619=ORIENTED_EDGE('',*,*,#3130,.F.);
#4620=ORIENTED_EDGE('',*,*,#3133,.F.);
#4621=ORIENTED_EDGE('',*,*,#3132,.T.);
#4622=ORIENTED_EDGE('',*,*,#3136,.T.);
#4623=ORIENTED_EDGE('',*,*,#3137,.T.);
#4624=ORIENTED_EDGE('',*,*,#3138,.F.);
#4625=ORIENTED_EDGE('',*,*,#3137,.F.);
#4626=ORIENTED_EDGE('',*,*,#3139,.T.);
#4627=ORIENTED_EDGE('',*,*,#3140,.T.);
#4628=ORIENTED_EDGE('',*,*,#3141,.T.);
#4629=ORIENTED_EDGE('',*,*,#3142,.T.);
#4630=ORIENTED_EDGE('',*,*,#3143,.T.);
#4631=ORIENTED_EDGE('',*,*,#3144,.T.);
#4632=ORIENTED_EDGE('',*,*,#3136,.F.);
#4633=ORIENTED_EDGE('',*,*,#3145,.T.);
#4634=ORIENTED_EDGE('',*,*,#3146,.F.);
#4635=ORIENTED_EDGE('',*,*,#3139,.F.);
#4636=ORIENTED_EDGE('',*,*,#3147,.T.);
#4637=ORIENTED_EDGE('',*,*,#3148,.T.);
#4638=ORIENTED_EDGE('',*,*,#3149,.F.);
#4639=ORIENTED_EDGE('',*,*,#3140,.F.);
#4640=ORIENTED_EDGE('',*,*,#3146,.T.);
#4641=ORIENTED_EDGE('',*,*,#3150,.T.);
#4642=ORIENTED_EDGE('',*,*,#3151,.F.);
#4643=ORIENTED_EDGE('',*,*,#3141,.F.);
#4644=ORIENTED_EDGE('',*,*,#3149,.T.);
#4645=ORIENTED_EDGE('',*,*,#3152,.T.);
#4646=ORIENTED_EDGE('',*,*,#3153,.F.);
#4647=ORIENTED_EDGE('',*,*,#3142,.F.);
#4648=ORIENTED_EDGE('',*,*,#3151,.T.);
#4649=ORIENTED_EDGE('',*,*,#3154,.T.);
#4650=ORIENTED_EDGE('',*,*,#3155,.F.);
#4651=ORIENTED_EDGE('',*,*,#3143,.F.);
#4652=ORIENTED_EDGE('',*,*,#3153,.T.);
#4653=ORIENTED_EDGE('',*,*,#3156,.T.);
#4654=ORIENTED_EDGE('',*,*,#3147,.F.);
#4655=ORIENTED_EDGE('',*,*,#3144,.F.);
#4656=ORIENTED_EDGE('',*,*,#3155,.T.);
#4657=ORIENTED_EDGE('',*,*,#3145,.F.);
#4658=ORIENTED_EDGE('',*,*,#3156,.F.);
#4659=ORIENTED_EDGE('',*,*,#3154,.F.);
#4660=ORIENTED_EDGE('',*,*,#3152,.F.);
#4661=ORIENTED_EDGE('',*,*,#3150,.F.);
#4662=ORIENTED_EDGE('',*,*,#3148,.F.);
#4663=ORIENTED_EDGE('',*,*,#3138,.T.);
#4664=ORIENTED_EDGE('',*,*,#3157,.T.);
#4665=ORIENTED_EDGE('',*,*,#3158,.T.);
#4666=ORIENTED_EDGE('',*,*,#3159,.T.);
#4667=ORIENTED_EDGE('',*,*,#3160,.F.);
#4668=ORIENTED_EDGE('',*,*,#3161,.T.);
#4669=ORIENTED_EDGE('',*,*,#3162,.T.);
#4670=ORIENTED_EDGE('',*,*,#3157,.F.);
#4671=ORIENTED_EDGE('',*,*,#3163,.F.);
#4672=ORIENTED_EDGE('',*,*,#3164,.T.);
#4673=ORIENTED_EDGE('',*,*,#3165,.T.);
#4674=ORIENTED_EDGE('',*,*,#3161,.F.);
#4675=ORIENTED_EDGE('',*,*,#3166,.F.);
#4676=ORIENTED_EDGE('',*,*,#3167,.F.);
#4677=ORIENTED_EDGE('',*,*,#3168,.F.);
#4678=ORIENTED_EDGE('',*,*,#3169,.T.);
#4679=ORIENTED_EDGE('',*,*,#3170,.T.);
#4680=ORIENTED_EDGE('',*,*,#3171,.F.);
#4681=ORIENTED_EDGE('',*,*,#3172,.F.);
#4682=ORIENTED_EDGE('',*,*,#3173,.T.);
#4683=ORIENTED_EDGE('',*,*,#3174,.T.);
#4684=ORIENTED_EDGE('',*,*,#3175,.F.);
#4685=ORIENTED_EDGE('',*,*,#3176,.T.);
#4686=ORIENTED_EDGE('',*,*,#3177,.T.);
#4687=ORIENTED_EDGE('',*,*,#3178,.T.);
#4688=ORIENTED_EDGE('',*,*,#3179,.F.);
#4689=ORIENTED_EDGE('',*,*,#3180,.T.);
#4690=ORIENTED_EDGE('',*,*,#3181,.F.);
#4691=ORIENTED_EDGE('',*,*,#3172,.T.);
#4692=ORIENTED_EDGE('',*,*,#3182,.T.);
#4693=ORIENTED_EDGE('',*,*,#3183,.T.);
#4694=ORIENTED_EDGE('',*,*,#3184,.F.);
#4695=ORIENTED_EDGE('',*,*,#3180,.F.);
#4696=ORIENTED_EDGE('',*,*,#3185,.T.);
#4697=ORIENTED_EDGE('',*,*,#3186,.F.);
#4698=ORIENTED_EDGE('',*,*,#3187,.T.);
#4699=ORIENTED_EDGE('',*,*,#3177,.F.);
#4700=ORIENTED_EDGE('',*,*,#3188,.F.);
#4701=ORIENTED_EDGE('',*,*,#3186,.T.);
#4702=ORIENTED_EDGE('',*,*,#3189,.F.);
#4703=ORIENTED_EDGE('',*,*,#3183,.F.);
#4704=ORIENTED_EDGE('',*,*,#3190,.T.);
#4705=ORIENTED_EDGE('',*,*,#3191,.F.);
#4706=ORIENTED_EDGE('',*,*,#3192,.F.);
#4707=ORIENTED_EDGE('',*,*,#3193,.F.);
#4708=ORIENTED_EDGE('',*,*,#3194,.F.);
#4709=ORIENTED_EDGE('',*,*,#3195,.T.);
#4710=ORIENTED_EDGE('',*,*,#3196,.F.);
#4711=ORIENTED_EDGE('',*,*,#3195,.F.);
#4712=ORIENTED_EDGE('',*,*,#3197,.F.);
#4713=ORIENTED_EDGE('',*,*,#3198,.F.);
#4714=ORIENTED_EDGE('',*,*,#3199,.F.);
#4715=ORIENTED_EDGE('',*,*,#3175,.T.);
#4716=ORIENTED_EDGE('',*,*,#3200,.F.);
#4717=ORIENTED_EDGE('',*,*,#3201,.T.);
#4718=ORIENTED_EDGE('',*,*,#3171,.T.);
#4719=ORIENTED_EDGE('',*,*,#3202,.T.);
#4720=ORIENTED_EDGE('',*,*,#3203,.T.);
#4721=ORIENTED_EDGE('',*,*,#3204,.T.);
#4722=ORIENTED_EDGE('',*,*,#3205,.T.);
#4723=ORIENTED_EDGE('',*,*,#3206,.T.);
#4724=ORIENTED_EDGE('',*,*,#3207,.T.);
#4725=ORIENTED_EDGE('',*,*,#3208,.T.);
#4726=ORIENTED_EDGE('',*,*,#3209,.T.);
#4727=ORIENTED_EDGE('',*,*,#3210,.F.);
#4728=ORIENTED_EDGE('',*,*,#3159,.F.);
#4729=ORIENTED_EDGE('',*,*,#3211,.F.);
#4730=ORIENTED_EDGE('',*,*,#3200,.T.);
#4731=ORIENTED_EDGE('',*,*,#3179,.T.);
#4732=ORIENTED_EDGE('',*,*,#3196,.T.);
#4733=ORIENTED_EDGE('',*,*,#3212,.F.);
#4734=ORIENTED_EDGE('',*,*,#3202,.F.);
#4735=ORIENTED_EDGE('',*,*,#3174,.F.);
#4736=ORIENTED_EDGE('',*,*,#3213,.F.);
#4737=ORIENTED_EDGE('',*,*,#3169,.F.);
#4738=ORIENTED_EDGE('',*,*,#3198,.T.);
#4739=ORIENTED_EDGE('',*,*,#3214,.T.);
#4740=ORIENTED_EDGE('',*,*,#3204,.F.);
#4741=ORIENTED_EDGE('',*,*,#3215,.F.);
#4742=ORIENTED_EDGE('',*,*,#3199,.T.);
#4743=ORIENTED_EDGE('',*,*,#3215,.T.);
#4744=ORIENTED_EDGE('',*,*,#3209,.F.);
#4745=ORIENTED_EDGE('',*,*,#3216,.F.);
#4746=ORIENTED_EDGE('',*,*,#3191,.T.);
#4747=ORIENTED_EDGE('',*,*,#3216,.T.);
#4748=ORIENTED_EDGE('',*,*,#3208,.F.);
#4749=ORIENTED_EDGE('',*,*,#3217,.F.);
#4750=ORIENTED_EDGE('',*,*,#3192,.T.);
#4751=ORIENTED_EDGE('',*,*,#3217,.T.);
#4752=ORIENTED_EDGE('',*,*,#3207,.F.);
#4753=ORIENTED_EDGE('',*,*,#3218,.F.);
#4754=ORIENTED_EDGE('',*,*,#3193,.T.);
#4755=ORIENTED_EDGE('',*,*,#3218,.T.);
#4756=ORIENTED_EDGE('',*,*,#3206,.F.);
#4757=ORIENTED_EDGE('',*,*,#3219,.F.);
#4758=ORIENTED_EDGE('',*,*,#3197,.T.);
#4759=ORIENTED_EDGE('',*,*,#3194,.T.);
#4760=ORIENTED_EDGE('',*,*,#3219,.T.);
#4761=ORIENTED_EDGE('',*,*,#3205,.F.);
#4762=ORIENTED_EDGE('',*,*,#3214,.F.);
#4763=ORIENTED_EDGE('',*,*,#3167,.T.);
#4764=ORIENTED_EDGE('',*,*,#3220,.T.);
#4765=ORIENTED_EDGE('',*,*,#3164,.F.);
#4766=ORIENTED_EDGE('',*,*,#3221,.F.);
#4767=ORIENTED_EDGE('',*,*,#3212,.T.);
#4768=ORIENTED_EDGE('',*,*,#3168,.T.);
#4769=ORIENTED_EDGE('',*,*,#3221,.T.);
#4770=ORIENTED_EDGE('',*,*,#3166,.T.);
#4771=ORIENTED_EDGE('',*,*,#3163,.T.);
#4772=ORIENTED_EDGE('',*,*,#3160,.T.);
#4773=ORIENTED_EDGE('',*,*,#3210,.T.);
#4774=ORIENTED_EDGE('',*,*,#3178,.F.);
#4775=ORIENTED_EDGE('',*,*,#3187,.F.);
#4776=ORIENTED_EDGE('',*,*,#3190,.F.);
#4777=ORIENTED_EDGE('',*,*,#3185,.F.);
#4778=ORIENTED_EDGE('',*,*,#3182,.F.);
#4779=ORIENTED_EDGE('',*,*,#3203,.F.);
#4780=ORIENTED_EDGE('',*,*,#3213,.T.);
#4781=ORIENTED_EDGE('',*,*,#3173,.F.);
#4782=ORIENTED_EDGE('',*,*,#3181,.T.);
#4783=ORIENTED_EDGE('',*,*,#3184,.T.);
#4784=ORIENTED_EDGE('',*,*,#3189,.T.);
#4785=ORIENTED_EDGE('',*,*,#3188,.T.);
#4786=ORIENTED_EDGE('',*,*,#3176,.F.);
#4787=ORIENTED_EDGE('',*,*,#3201,.F.);
#4788=ORIENTED_EDGE('',*,*,#3211,.T.);
#4789=ORIENTED_EDGE('',*,*,#3158,.F.);
#4790=ORIENTED_EDGE('',*,*,#3162,.F.);
#4791=ORIENTED_EDGE('',*,*,#3165,.F.);
#4792=ORIENTED_EDGE('',*,*,#3220,.F.);
#4793=ORIENTED_EDGE('',*,*,#3170,.F.);
#4794=CYLINDRICAL_SURFACE('',#5398,3.);
#4795=CYLINDRICAL_SURFACE('',#5401,3.);
#4796=CYLINDRICAL_SURFACE('',#5404,8.5);
#4797=CYLINDRICAL_SURFACE('',#5407,9.5);
#4798=CYLINDRICAL_SURFACE('',#5410,9.5);
#4799=CYLINDRICAL_SURFACE('',#5413,2.99999999999929);
#4800=CYLINDRICAL_SURFACE('',#5416,3.);
#4801=CYLINDRICAL_SURFACE('',#5419,2.99999999999976);
#4802=CYLINDRICAL_SURFACE('',#5422,3.);
#4803=CYLINDRICAL_SURFACE('',#5436,4.);
#4804=CYLINDRICAL_SURFACE('',#5439,4.5);
#4805=CYLINDRICAL_SURFACE('',#5444,5.);
#4806=CYLINDRICAL_SURFACE('',#5449,6.);
#4807=CYLINDRICAL_SURFACE('',#5452,5.);
#4808=CYLINDRICAL_SURFACE('',#5467,4.5);
#4809=CYLINDRICAL_SURFACE('',#5470,0.405000000000001);
#4810=CYLINDRICAL_SURFACE('',#5473,5.53127226019911);
#4811=CYLINDRICAL_SURFACE('',#5476,0.404999999999999);
#4812=CYLINDRICAL_SURFACE('',#5479,5.53127226019911);
#4813=CYLINDRICAL_SURFACE('',#5482,0.405);
#4814=CYLINDRICAL_SURFACE('',#5485,5.53127226019911);
#4815=CYLINDRICAL_SURFACE('',#5488,0.404999999999999);
#4816=CYLINDRICAL_SURFACE('',#5491,5.53127226019911);
#4817=CYLINDRICAL_SURFACE('',#5494,0.404999999999999);
#4818=CYLINDRICAL_SURFACE('',#5497,0.404999999999999);
#4819=CYLINDRICAL_SURFACE('',#5500,0.404999999999999);
#4820=CYLINDRICAL_SURFACE('',#5503,0.404999999999999);
#4821=CYLINDRICAL_SURFACE('',#5506,0.404999999999999);
#4822=CYLINDRICAL_SURFACE('',#5509,0.404999999999999);
#4823=CYLINDRICAL_SURFACE('',#5512,0.404999999999999);
#4824=CYLINDRICAL_SURFACE('',#5515,0.404999999999999);
#4825=CYLINDRICAL_SURFACE('',#5518,0.404999999999999);
#4826=CYLINDRICAL_SURFACE('',#5521,0.404999999999999);
#4827=CYLINDRICAL_SURFACE('',#5524,21.6);
#4828=CYLINDRICAL_SURFACE('',#5527,21.6);
#4829=CYLINDRICAL_SURFACE('',#5530,21.6);
#4830=CYLINDRICAL_SURFACE('',#5533,21.6);
#4831=CYLINDRICAL_SURFACE('',#5536,21.6);
#4832=CYLINDRICAL_SURFACE('',#5539,21.6);
#4833=CYLINDRICAL_SURFACE('',#5542,21.6);
#4834=CYLINDRICAL_SURFACE('',#5545,21.6);
#4835=CYLINDRICAL_SURFACE('',#5548,21.6);
#4836=CYLINDRICAL_SURFACE('',#5551,21.6);
#4837=CYLINDRICAL_SURFACE('',#5554,21.6);
#4838=CYLINDRICAL_SURFACE('',#5557,21.6);
#4839=CYLINDRICAL_SURFACE('',#5560,21.6);
#4840=CYLINDRICAL_SURFACE('',#5563,21.6);
#4841=CYLINDRICAL_SURFACE('',#5566,21.6);
#4842=CYLINDRICAL_SURFACE('',#5569,21.6);
#4843=CYLINDRICAL_SURFACE('',#5572,21.6);
#4844=CYLINDRICAL_SURFACE('',#5575,21.6);
#4845=CYLINDRICAL_SURFACE('',#5578,21.6);
#4846=CYLINDRICAL_SURFACE('',#5581,21.6);
#4847=CYLINDRICAL_SURFACE('',#5584,21.6);
#4848=CYLINDRICAL_SURFACE('',#5587,21.6);
#4849=CYLINDRICAL_SURFACE('',#5590,21.6);
#4850=CYLINDRICAL_SURFACE('',#5593,21.6);
#4851=CYLINDRICAL_SURFACE('',#5596,21.6);
#4852=CYLINDRICAL_SURFACE('',#5599,21.6);
#4853=CYLINDRICAL_SURFACE('',#5602,21.6);
#4854=CYLINDRICAL_SURFACE('',#5605,21.6);
#4855=CYLINDRICAL_SURFACE('',#5608,21.6);
#4856=CYLINDRICAL_SURFACE('',#5879,21.6);
#4857=CYLINDRICAL_SURFACE('',#5880,5.53127226019911);
#4858=CYLINDRICAL_SURFACE('',#5881,5.53127226019911);
#4859=CYLINDRICAL_SURFACE('',#5882,18.5625);
#4860=CYLINDRICAL_SURFACE('',#5883,0.405);
#4861=CYLINDRICAL_SURFACE('',#5884,0.405);
#4862=CYLINDRICAL_SURFACE('',#5885,5.53127226019911);
#4863=CYLINDRICAL_SURFACE('',#5886,5.53127226019911);
#4864=CYLINDRICAL_SURFACE('',#5887,0.405);
#4865=CYLINDRICAL_SURFACE('',#5888,18.5625);
#4866=CYLINDRICAL_SURFACE('',#5889,0.405000000000001);
#4867=CYLINDRICAL_SURFACE('',#5890,5.53127226019911);
#4868=CYLINDRICAL_SURFACE('',#5891,5.53127226019911);
#4869=CYLINDRICAL_SURFACE('',#5892,0.404999999999999);
#4870=CYLINDRICAL_SURFACE('',#5893,18.5625);
#4871=CYLINDRICAL_SURFACE('',#5894,5.53127226019911);
#4872=CYLINDRICAL_SURFACE('',#5895,5.53127226019911);
#4873=CYLINDRICAL_SURFACE('',#5896,0.404999999999999);
#4874=CYLINDRICAL_SURFACE('',#5897,18.5625);
#4875=CYLINDRICAL_SURFACE('',#5898,5.53127226019911);
#4876=CYLINDRICAL_SURFACE('',#5899,5.53127226019911);
#4877=CYLINDRICAL_SURFACE('',#5900,0.404999999999999);
#4878=CYLINDRICAL_SURFACE('',#5901,18.5625);
#4879=CYLINDRICAL_SURFACE('',#5902,5.53127226019911);
#4880=CYLINDRICAL_SURFACE('',#5903,5.53127226019911);
#4881=CYLINDRICAL_SURFACE('',#5904,0.404999999999999);
#4882=CYLINDRICAL_SURFACE('',#5905,18.5625);
#4883=CYLINDRICAL_SURFACE('',#5906,5.53127226019911);
#4884=CYLINDRICAL_SURFACE('',#5907,5.53127226019911);
#4885=CYLINDRICAL_SURFACE('',#5908,0.404999999999999);
#4886=CYLINDRICAL_SURFACE('',#5909,18.5625);
#4887=CYLINDRICAL_SURFACE('',#5910,5.53127226019911);
#4888=CYLINDRICAL_SURFACE('',#5911,5.53127226019911);
#4889=CYLINDRICAL_SURFACE('',#5912,18.5625);
#4890=CYLINDRICAL_SURFACE('',#5913,0.404999999999999);
#4891=CYLINDRICAL_SURFACE('',#5914,5.53127226019911);
#4892=CYLINDRICAL_SURFACE('',#5915,5.53127226019911);
#4893=CYLINDRICAL_SURFACE('',#5916,18.5625);
#4894=CYLINDRICAL_SURFACE('',#5917,0.404999999999999);
#4895=CYLINDRICAL_SURFACE('',#5918,5.53127226019911);
#4896=CYLINDRICAL_SURFACE('',#5919,5.53127226019911);
#4897=CYLINDRICAL_SURFACE('',#5920,18.5625);
#4898=CYLINDRICAL_SURFACE('',#5921,0.404999999999999);
#4899=CYLINDRICAL_SURFACE('',#5922,5.53127226019911);
#4900=CYLINDRICAL_SURFACE('',#5923,5.53127226019911);
#4901=CYLINDRICAL_SURFACE('',#5924,18.5625);
#4902=CYLINDRICAL_SURFACE('',#5925,0.404999999999999);
#4903=CYLINDRICAL_SURFACE('',#5926,5.53127226019911);
#4904=CYLINDRICAL_SURFACE('',#5927,5.53127226019911);
#4905=CYLINDRICAL_SURFACE('',#5928,18.5625);
#4906=CYLINDRICAL_SURFACE('',#5929,0.404999999999999);
#4907=CYLINDRICAL_SURFACE('',#5930,5.53127226019911);
#4908=CYLINDRICAL_SURFACE('',#5931,18.5625);
#4909=CYLINDRICAL_SURFACE('',#5932,0.404999999999999);
#4910=CYLINDRICAL_SURFACE('',#5933,5.53127226019911);
#4911=CYLINDRICAL_SURFACE('',#5934,18.5625);
#4912=CYLINDRICAL_SURFACE('',#5935,0.405000000000001);
#4913=CYLINDRICAL_SURFACE('',#5936,5.53127226019911);
#4914=CYLINDRICAL_SURFACE('',#5937,0.405000000000001);
#4915=CYLINDRICAL_SURFACE('',#5938,18.5625);
#4916=CYLINDRICAL_SURFACE('',#5939,5.53127226019911);
#4917=CYLINDRICAL_SURFACE('',#5940,0.405);
#4918=CYLINDRICAL_SURFACE('',#5941,18.5625);
#4919=CYLINDRICAL_SURFACE('',#5942,5.53127226019911);
#4920=CYLINDRICAL_SURFACE('',#5943,5.53127226019911);
#4921=CYLINDRICAL_SURFACE('',#5944,0.405);
#4922=CYLINDRICAL_SURFACE('',#5945,18.5625);
#4923=CYLINDRICAL_SURFACE('',#5946,0.405);
#4924=CYLINDRICAL_SURFACE('',#5947,5.53127226019911);
#4925=CYLINDRICAL_SURFACE('',#5948,5.53127226019911);
#4926=CYLINDRICAL_SURFACE('',#5949,0.405);
#4927=CYLINDRICAL_SURFACE('',#5950,18.5625);
#4928=CYLINDRICAL_SURFACE('',#5951,0.404999999999999);
#4929=CYLINDRICAL_SURFACE('',#5952,5.53127226019911);
#4930=CYLINDRICAL_SURFACE('',#5953,5.53127226019911);
#4931=CYLINDRICAL_SURFACE('',#5954,0.404999999999999);
#4932=CYLINDRICAL_SURFACE('',#5955,18.5625);
#4933=CYLINDRICAL_SURFACE('',#5956,0.404999999999999);
#4934=CYLINDRICAL_SURFACE('',#5957,5.53127226019911);
#4935=CYLINDRICAL_SURFACE('',#5958,5.53127226019911);
#4936=CYLINDRICAL_SURFACE('',#5959,0.404999999999999);
#4937=CYLINDRICAL_SURFACE('',#5960,18.5625);
#4938=CYLINDRICAL_SURFACE('',#5961,0.404999999999999);
#4939=CYLINDRICAL_SURFACE('',#5962,5.53127226019911);
#4940=CYLINDRICAL_SURFACE('',#5963,5.53127226019911);
#4941=CYLINDRICAL_SURFACE('',#5964,0.404999999999999);
#4942=CYLINDRICAL_SURFACE('',#5965,18.5625);
#4943=CYLINDRICAL_SURFACE('',#5966,0.404999999999999);
#4944=CYLINDRICAL_SURFACE('',#5967,5.53127226019911);
#4945=CYLINDRICAL_SURFACE('',#5968,5.53127226019911);
#4946=CYLINDRICAL_SURFACE('',#5969,0.405000000000001);
#4947=CYLINDRICAL_SURFACE('',#5970,18.5625);
#4948=CYLINDRICAL_SURFACE('',#5971,0.404999999999999);
#4949=CYLINDRICAL_SURFACE('',#5972,5.53127226019911);
#4950=CYLINDRICAL_SURFACE('',#5973,5.53127226019911);
#4951=CYLINDRICAL_SURFACE('',#5974,0.404999999999999);
#4952=CYLINDRICAL_SURFACE('',#5975,18.5625);
#4953=CYLINDRICAL_SURFACE('',#5976,0.404999999999999);
#4954=CYLINDRICAL_SURFACE('',#5977,5.53127226019911);
#4955=CYLINDRICAL_SURFACE('',#5978,5.53127226019911);
#4956=CYLINDRICAL_SURFACE('',#5979,0.404999999999999);
#4957=CYLINDRICAL_SURFACE('',#5980,18.5625);
#4958=CYLINDRICAL_SURFACE('',#5981,0.404999999999999);
#4959=CYLINDRICAL_SURFACE('',#5982,5.53127226019912);
#4960=CYLINDRICAL_SURFACE('',#5983,5.53127226019911);
#4961=CYLINDRICAL_SURFACE('',#5984,0.404999999999999);
#4962=CYLINDRICAL_SURFACE('',#5985,18.5625);
#4963=CYLINDRICAL_SURFACE('',#5986,0.404999999999999);
#4964=CYLINDRICAL_SURFACE('',#5987,5.53127226019911);
#4965=CYLINDRICAL_SURFACE('',#5988,5.53127226019911);
#4966=CYLINDRICAL_SURFACE('',#5989,0.404999999999999);
#4967=CYLINDRICAL_SURFACE('',#5990,18.5625);
#4968=CYLINDRICAL_SURFACE('',#5991,0.404999999999999);
#4969=CYLINDRICAL_SURFACE('',#5992,5.53127226019911);
#4970=CYLINDRICAL_SURFACE('',#5993,5.53127226019911);
#4971=CYLINDRICAL_SURFACE('',#5994,0.404999999999999);
#4972=CYLINDRICAL_SURFACE('',#5995,18.5625);
#4973=CYLINDRICAL_SURFACE('',#5996,0.404999999999999);
#4974=CYLINDRICAL_SURFACE('',#5997,5.53127226019911);
#4975=CYLINDRICAL_SURFACE('',#5998,5.53127226019911);
#4976=CYLINDRICAL_SURFACE('',#5999,0.404999999999999);
#4977=CYLINDRICAL_SURFACE('',#6000,18.5625);
#4978=CYLINDRICAL_SURFACE('',#6001,0.404999999999999);
#4979=CYLINDRICAL_SURFACE('',#6002,5.53127226019911);
#4980=CYLINDRICAL_SURFACE('',#6003,5.53127226019911);
#4981=CYLINDRICAL_SURFACE('',#6004,0.404999999999999);
#4982=CYLINDRICAL_SURFACE('',#6005,18.5625);
#4983=CYLINDRICAL_SURFACE('',#6006,0.404999999999999);
#4984=CYLINDRICAL_SURFACE('',#6007,5.53127226019911);
#4985=CYLINDRICAL_SURFACE('',#6008,5.53127226019911);
#4986=CYLINDRICAL_SURFACE('',#6009,0.404999999999999);
#4987=CYLINDRICAL_SURFACE('',#6010,18.5625);
#4988=CYLINDRICAL_SURFACE('',#6011,0.404999999999999);
#4989=CYLINDRICAL_SURFACE('',#6016,3.4);
#4990=CYLINDRICAL_SURFACE('',#6052,8.);
#4991=CYLINDRICAL_SURFACE('',#6055,25.);
#4992=CYLINDRICAL_SURFACE('',#6058,3.);
#4993=CYLINDRICAL_SURFACE('',#6061,3.);
#4994=CYLINDRICAL_SURFACE('',#6064,3.);
#4995=CYLINDRICAL_SURFACE('',#6067,3.);
#4996=CYLINDRICAL_SURFACE('',#6070,9.5);
#4997=CYLINDRICAL_SURFACE('',#6077,5.);
#4998=CYLINDRICAL_SURFACE('',#6080,9.5);
#4999=CYLINDRICAL_SURFACE('',#6086,2.5);
#5000=CYLINDRICAL_SURFACE('',#6099,2.54979787499999);
#5001=CYLINDRICAL_SURFACE('',#6101,2.54979787499999);
#5002=CYLINDRICAL_SURFACE('',#6102,2.54979787499999);
#5003=CYLINDRICAL_SURFACE('',#6103,2.54979787499999);
#5004=CYLINDRICAL_SURFACE('',#6111,2.008532);
#5005=CYLINDRICAL_SURFACE('',#6112,2.008532);
#5006=CYLINDRICAL_SURFACE('',#6113,2.008532);
#5007=CYLINDRICAL_SURFACE('',#6114,2.008532);
#5008=CYLINDRICAL_SURFACE('',#6133,2.54979787499999);
#5009=ADVANCED_FACE('',(#275),#4794,.F.);
#5010=ADVANCED_FACE('',(#276),#4795,.F.);
#5011=ADVANCED_FACE('',(#277),#4796,.F.);
#5012=ADVANCED_FACE('',(#278),#4797,.F.);
#5013=ADVANCED_FACE('',(#279),#4798,.F.);
#5014=ADVANCED_FACE('',(#280),#4799,.F.);
#5015=ADVANCED_FACE('',(#281),#4800,.F.);
#5016=ADVANCED_FACE('',(#282),#4801,.F.);
#5017=ADVANCED_FACE('',(#283),#4802,.F.);
#5018=ADVANCED_FACE('',(#284,#180,#181,#182,#183,#184),#219,.F.);
#5019=ADVANCED_FACE('',(#285,#185,#186,#187,#188,#189),#220,.T.);
#5020=ADVANCED_FACE('',(#286),#221,.F.);
#5021=ADVANCED_FACE('',(#287),#222,.F.);
#5022=ADVANCED_FACE('',(#288,#190),#223,.T.);
#5023=ADVANCED_FACE('',(#289,#191),#224,.T.);
#5024=ADVANCED_FACE('',(#290),#225,.F.);
#5025=ADVANCED_FACE('',(#291,#192,#193),#226,.T.);
#5026=ADVANCED_FACE('',(#292,#194,#195),#227,.F.);
#5027=ADVANCED_FACE('',(#293),#228,.F.);
#5028=ADVANCED_FACE('',(#294),#4803,.T.);
#5029=ADVANCED_FACE('',(#295),#4804,.T.);
#5030=ADVANCED_FACE('',(#296),#4805,.T.);
#5031=ADVANCED_FACE('',(#297),#4806,.T.);
#5032=ADVANCED_FACE('',(#298),#4807,.T.);
#5033=ADVANCED_FACE('',(#299,#196),#229,.T.);
#5034=ADVANCED_FACE('',(#300,#197),#230,.T.);
#5035=ADVANCED_FACE('',(#301),#231,.F.);
#5036=ADVANCED_FACE('',(#302,#198),#232,.F.);
#5037=ADVANCED_FACE('',(#303),#233,.T.);
#5038=ADVANCED_FACE('',(#304),#234,.F.);
#5039=ADVANCED_FACE('',(#305),#235,.F.);
#5040=ADVANCED_FACE('',(#306),#236,.F.);
#5041=ADVANCED_FACE('',(#307),#237,.F.);
#5042=ADVANCED_FACE('',(#308),#238,.T.);
#5043=ADVANCED_FACE('',(#309),#239,.T.);
#5044=ADVANCED_FACE('',(#310),#4808,.F.);
#5045=ADVANCED_FACE('',(#311),#4809,.F.);
#5046=ADVANCED_FACE('',(#312),#4810,.T.);
#5047=ADVANCED_FACE('',(#313),#4811,.F.);
#5048=ADVANCED_FACE('',(#314),#4812,.T.);
#5049=ADVANCED_FACE('',(#315),#4813,.F.);
#5050=ADVANCED_FACE('',(#316),#4814,.T.);
#5051=ADVANCED_FACE('',(#317),#4815,.F.);
#5052=ADVANCED_FACE('',(#318),#4816,.T.);
#5053=ADVANCED_FACE('',(#319),#4817,.F.);
#5054=ADVANCED_FACE('',(#320),#4818,.F.);
#5055=ADVANCED_FACE('',(#321),#4819,.F.);
#5056=ADVANCED_FACE('',(#322),#4820,.F.);
#5057=ADVANCED_FACE('',(#323),#4821,.F.);
#5058=ADVANCED_FACE('',(#324),#4822,.F.);
#5059=ADVANCED_FACE('',(#325),#4823,.F.);
#5060=ADVANCED_FACE('',(#326),#4824,.F.);
#5061=ADVANCED_FACE('',(#327),#4825,.F.);
#5062=ADVANCED_FACE('',(#328),#4826,.F.);
#5063=ADVANCED_FACE('',(#329),#4827,.T.);
#5064=ADVANCED_FACE('',(#330),#4828,.T.);
#5065=ADVANCED_FACE('',(#331),#4829,.T.);
#5066=ADVANCED_FACE('',(#332),#4830,.T.);
#5067=ADVANCED_FACE('',(#333),#4831,.T.);
#5068=ADVANCED_FACE('',(#334),#4832,.T.);
#5069=ADVANCED_FACE('',(#335),#4833,.T.);
#5070=ADVANCED_FACE('',(#336),#4834,.T.);
#5071=ADVANCED_FACE('',(#337),#4835,.T.);
#5072=ADVANCED_FACE('',(#338),#4836,.T.);
#5073=ADVANCED_FACE('',(#339),#4837,.T.);
#5074=ADVANCED_FACE('',(#340),#4838,.T.);
#5075=ADVANCED_FACE('',(#341),#4839,.T.);
#5076=ADVANCED_FACE('',(#342),#4840,.T.);
#5077=ADVANCED_FACE('',(#343),#4841,.T.);
#5078=ADVANCED_FACE('',(#344),#4842,.T.);
#5079=ADVANCED_FACE('',(#345),#4843,.T.);
#5080=ADVANCED_FACE('',(#346),#4844,.T.);
#5081=ADVANCED_FACE('',(#347),#4845,.T.);
#5082=ADVANCED_FACE('',(#348),#4846,.T.);
#5083=ADVANCED_FACE('',(#349),#4847,.T.);
#5084=ADVANCED_FACE('',(#350),#4848,.T.);
#5085=ADVANCED_FACE('',(#351),#4849,.T.);
#5086=ADVANCED_FACE('',(#352),#4850,.T.);
#5087=ADVANCED_FACE('',(#353),#4851,.T.);
#5088=ADVANCED_FACE('',(#354),#4852,.T.);
#5089=ADVANCED_FACE('',(#355),#4853,.T.);
#5090=ADVANCED_FACE('',(#356),#4854,.T.);
#5091=ADVANCED_FACE('',(#357),#4855,.T.);
#5092=ADVANCED_FACE('',(#358,#199),#240,.F.);
#5093=ADVANCED_FACE('',(#359,#200),#241,.T.);
#5094=ADVANCED_FACE('',(#360),#4856,.T.);
#5095=ADVANCED_FACE('',(#361),#4857,.T.);
#5096=ADVANCED_FACE('',(#362),#4858,.T.);
#5097=ADVANCED_FACE('',(#363),#4859,.T.);
#5098=ADVANCED_FACE('',(#364),#4860,.F.);
#5099=ADVANCED_FACE('',(#365),#4861,.F.);
#5100=ADVANCED_FACE('',(#366),#4862,.T.);
#5101=ADVANCED_FACE('',(#367),#4863,.T.);
#5102=ADVANCED_FACE('',(#368),#4864,.F.);
#5103=ADVANCED_FACE('',(#369),#4865,.T.);
#5104=ADVANCED_FACE('',(#370),#4866,.F.);
#5105=ADVANCED_FACE('',(#371),#4867,.T.);
#5106=ADVANCED_FACE('',(#372),#4868,.T.);
#5107=ADVANCED_FACE('',(#373),#4869,.F.);
#5108=ADVANCED_FACE('',(#374),#4870,.T.);
#5109=ADVANCED_FACE('',(#375),#4871,.T.);
#5110=ADVANCED_FACE('',(#376),#4872,.T.);
#5111=ADVANCED_FACE('',(#377),#4873,.F.);
#5112=ADVANCED_FACE('',(#378),#4874,.T.);
#5113=ADVANCED_FACE('',(#379),#4875,.T.);
#5114=ADVANCED_FACE('',(#380),#4876,.T.);
#5115=ADVANCED_FACE('',(#381),#4877,.F.);
#5116=ADVANCED_FACE('',(#382),#4878,.T.);
#5117=ADVANCED_FACE('',(#383),#4879,.T.);
#5118=ADVANCED_FACE('',(#384),#4880,.T.);
#5119=ADVANCED_FACE('',(#385),#4881,.F.);
#5120=ADVANCED_FACE('',(#386),#4882,.T.);
#5121=ADVANCED_FACE('',(#387),#4883,.T.);
#5122=ADVANCED_FACE('',(#388),#4884,.T.);
#5123=ADVANCED_FACE('',(#389),#4885,.F.);
#5124=ADVANCED_FACE('',(#390),#4886,.T.);
#5125=ADVANCED_FACE('',(#391),#4887,.T.);
#5126=ADVANCED_FACE('',(#392),#4888,.T.);
#5127=ADVANCED_FACE('',(#393),#4889,.T.);
#5128=ADVANCED_FACE('',(#394),#4890,.F.);
#5129=ADVANCED_FACE('',(#395),#4891,.T.);
#5130=ADVANCED_FACE('',(#396),#4892,.T.);
#5131=ADVANCED_FACE('',(#397),#4893,.T.);
#5132=ADVANCED_FACE('',(#398),#4894,.F.);
#5133=ADVANCED_FACE('',(#399),#4895,.T.);
#5134=ADVANCED_FACE('',(#400),#4896,.T.);
#5135=ADVANCED_FACE('',(#401),#4897,.T.);
#5136=ADVANCED_FACE('',(#402),#4898,.F.);
#5137=ADVANCED_FACE('',(#403),#4899,.T.);
#5138=ADVANCED_FACE('',(#404),#4900,.T.);
#5139=ADVANCED_FACE('',(#405),#4901,.T.);
#5140=ADVANCED_FACE('',(#406),#4902,.F.);
#5141=ADVANCED_FACE('',(#407),#4903,.T.);
#5142=ADVANCED_FACE('',(#408),#4904,.T.);
#5143=ADVANCED_FACE('',(#409),#4905,.T.);
#5144=ADVANCED_FACE('',(#410),#4906,.F.);
#5145=ADVANCED_FACE('',(#411),#4907,.T.);
#5146=ADVANCED_FACE('',(#412),#4908,.T.);
#5147=ADVANCED_FACE('',(#413),#4909,.F.);
#5148=ADVANCED_FACE('',(#414),#4910,.T.);
#5149=ADVANCED_FACE('',(#415),#4911,.T.);
#5150=ADVANCED_FACE('',(#416),#4912,.F.);
#5151=ADVANCED_FACE('',(#417),#4913,.T.);
#5152=ADVANCED_FACE('',(#418),#4914,.F.);
#5153=ADVANCED_FACE('',(#419),#4915,.T.);
#5154=ADVANCED_FACE('',(#420),#4916,.T.);
#5155=ADVANCED_FACE('',(#421),#4917,.F.);
#5156=ADVANCED_FACE('',(#422),#4918,.T.);
#5157=ADVANCED_FACE('',(#423),#4919,.T.);
#5158=ADVANCED_FACE('',(#424),#4920,.T.);
#5159=ADVANCED_FACE('',(#425),#4921,.F.);
#5160=ADVANCED_FACE('',(#426),#4922,.T.);
#5161=ADVANCED_FACE('',(#427),#4923,.F.);
#5162=ADVANCED_FACE('',(#428),#4924,.T.);
#5163=ADVANCED_FACE('',(#429),#4925,.T.);
#5164=ADVANCED_FACE('',(#430),#4926,.F.);
#5165=ADVANCED_FACE('',(#431),#4927,.T.);
#5166=ADVANCED_FACE('',(#432),#4928,.F.);
#5167=ADVANCED_FACE('',(#433),#4929,.T.);
#5168=ADVANCED_FACE('',(#434),#4930,.T.);
#5169=ADVANCED_FACE('',(#435),#4931,.F.);
#5170=ADVANCED_FACE('',(#436),#4932,.T.);
#5171=ADVANCED_FACE('',(#437),#4933,.F.);
#5172=ADVANCED_FACE('',(#438),#4934,.T.);
#5173=ADVANCED_FACE('',(#439),#4935,.T.);
#5174=ADVANCED_FACE('',(#440),#4936,.F.);
#5175=ADVANCED_FACE('',(#441),#4937,.T.);
#5176=ADVANCED_FACE('',(#442),#4938,.F.);
#5177=ADVANCED_FACE('',(#443),#4939,.T.);
#5178=ADVANCED_FACE('',(#444),#4940,.T.);
#5179=ADVANCED_FACE('',(#445),#4941,.F.);
#5180=ADVANCED_FACE('',(#446),#4942,.T.);
#5181=ADVANCED_FACE('',(#447),#4943,.F.);
#5182=ADVANCED_FACE('',(#448),#4944,.T.);
#5183=ADVANCED_FACE('',(#449),#4945,.T.);
#5184=ADVANCED_FACE('',(#450),#4946,.F.);
#5185=ADVANCED_FACE('',(#451),#4947,.T.);
#5186=ADVANCED_FACE('',(#452),#4948,.F.);
#5187=ADVANCED_FACE('',(#453),#4949,.T.);
#5188=ADVANCED_FACE('',(#454),#4950,.T.);
#5189=ADVANCED_FACE('',(#455),#4951,.F.);
#5190=ADVANCED_FACE('',(#456),#4952,.T.);
#5191=ADVANCED_FACE('',(#457),#4953,.F.);
#5192=ADVANCED_FACE('',(#458),#4954,.T.);
#5193=ADVANCED_FACE('',(#459),#4955,.T.);
#5194=ADVANCED_FACE('',(#460),#4956,.F.);
#5195=ADVANCED_FACE('',(#461),#4957,.T.);
#5196=ADVANCED_FACE('',(#462),#4958,.F.);
#5197=ADVANCED_FACE('',(#463),#4959,.T.);
#5198=ADVANCED_FACE('',(#464),#4960,.T.);
#5199=ADVANCED_FACE('',(#465),#4961,.F.);
#5200=ADVANCED_FACE('',(#466),#4962,.T.);
#5201=ADVANCED_FACE('',(#467),#4963,.F.);
#5202=ADVANCED_FACE('',(#468),#4964,.T.);
#5203=ADVANCED_FACE('',(#469),#4965,.T.);
#5204=ADVANCED_FACE('',(#470),#4966,.F.);
#5205=ADVANCED_FACE('',(#471),#4967,.T.);
#5206=ADVANCED_FACE('',(#472),#4968,.F.);
#5207=ADVANCED_FACE('',(#473),#4969,.T.);
#5208=ADVANCED_FACE('',(#474),#4970,.T.);
#5209=ADVANCED_FACE('',(#475),#4971,.F.);
#5210=ADVANCED_FACE('',(#476),#4972,.T.);
#5211=ADVANCED_FACE('',(#477),#4973,.F.);
#5212=ADVANCED_FACE('',(#478),#4974,.T.);
#5213=ADVANCED_FACE('',(#479),#4975,.T.);
#5214=ADVANCED_FACE('',(#480),#4976,.F.);
#5215=ADVANCED_FACE('',(#481),#4977,.T.);
#5216=ADVANCED_FACE('',(#482),#4978,.F.);
#5217=ADVANCED_FACE('',(#483),#4979,.T.);
#5218=ADVANCED_FACE('',(#484),#4980,.T.);
#5219=ADVANCED_FACE('',(#485),#4981,.F.);
#5220=ADVANCED_FACE('',(#486),#4982,.T.);
#5221=ADVANCED_FACE('',(#487),#4983,.F.);
#5222=ADVANCED_FACE('',(#488),#4984,.T.);
#5223=ADVANCED_FACE('',(#489),#4985,.T.);
#5224=ADVANCED_FACE('',(#490),#4986,.F.);
#5225=ADVANCED_FACE('',(#491),#4987,.T.);
#5226=ADVANCED_FACE('',(#492),#4988,.F.);
#5227=ADVANCED_FACE('',(#493),#242,.F.);
#5228=ADVANCED_FACE('',(#494),#243,.F.);
#5229=ADVANCED_FACE('',(#495),#244,.F.);
#5230=ADVANCED_FACE('',(#496),#4989,.F.);
#5231=ADVANCED_FACE('',(#497),#131,.T.);
#5232=ADVANCED_FACE('',(#498),#132,.T.);
#5233=ADVANCED_FACE('',(#499),#245,.F.);
#5234=ADVANCED_FACE('',(#500),#246,.F.);
#5235=ADVANCED_FACE('',(#501),#247,.F.);
#5236=ADVANCED_FACE('',(#502),#248,.F.);
#5237=ADVANCED_FACE('',(#503),#249,.F.);
#5238=ADVANCED_FACE('',(#504),#250,.F.);
#5239=ADVANCED_FACE('',(#505),#133,.T.);
#5240=ADVANCED_FACE('',(#506),#134,.T.);
#5241=ADVANCED_FACE('',(#507),#135,.T.);
#5242=ADVANCED_FACE('',(#508),#136,.T.);
#5243=ADVANCED_FACE('',(#509),#137,.T.);
#5244=ADVANCED_FACE('',(#510,#201),#251,.F.);
#5245=ADVANCED_FACE('',(#511),#138,.T.);
#5246=ADVANCED_FACE('',(#512),#139,.T.);
#5247=ADVANCED_FACE('',(#513),#140,.T.);
#5248=ADVANCED_FACE('',(#514),#141,.T.);
#5249=ADVANCED_FACE('',(#515),#142,.T.);
#5250=ADVANCED_FACE('',(#516,#202),#252,.T.);
#5251=ADVANCED_FACE('',(#517),#4990,.F.);
#5252=ADVANCED_FACE('',(#518),#4991,.T.);
#5253=ADVANCED_FACE('',(#519),#4992,.F.);
#5254=ADVANCED_FACE('',(#520),#4993,.F.);
#5255=ADVANCED_FACE('',(#521),#4994,.F.);
#5256=ADVANCED_FACE('',(#522),#4995,.F.);
#5257=ADVANCED_FACE('',(#523),#4996,.F.);
#5258=ADVANCED_FACE('',(#524,#203,#204,#205,#206,#207),#253,.T.);
#5259=ADVANCED_FACE('',(#525,#208,#209,#210,#211,#212),#254,.F.);
#5260=ADVANCED_FACE('',(#526,#213),#255,.T.);
#5261=ADVANCED_FACE('',(#527),#4997,.F.);
#5262=ADVANCED_FACE('',(#528),#4998,.T.);
#5263=ADVANCED_FACE('',(#529,#214),#256,.T.);
#5264=ADVANCED_FACE('',(#530,#215),#257,.F.);
#5265=ADVANCED_FACE('',(#531),#4999,.T.);
#5266=ADVANCED_FACE('',(#532,#216),#258,.T.);
#5267=ADVANCED_FACE('',(#533),#259,.F.);
#5268=ADVANCED_FACE('',(#534),#260,.F.);
#5269=ADVANCED_FACE('',(#535),#261,.F.);
#5270=ADVANCED_FACE('',(#536),#262,.F.);
#5271=ADVANCED_FACE('',(#537),#263,.F.);
#5272=ADVANCED_FACE('',(#538),#264,.F.);
#5273=ADVANCED_FACE('',(#539),#265,.F.);
#5274=ADVANCED_FACE('',(#540),#266,.T.);
#5275=ADVANCED_FACE('',(#541),#5000,.F.);
#5276=ADVANCED_FACE('',(#542),#5001,.F.);
#5277=ADVANCED_FACE('',(#543),#5002,.F.);
#5278=ADVANCED_FACE('',(#544),#5003,.F.);
#5279=ADVANCED_FACE('',(#545),#143,.F.);
#5280=ADVANCED_FACE('',(#546),#144,.F.);
#5281=ADVANCED_FACE('',(#547),#5004,.F.);
#5282=ADVANCED_FACE('',(#548),#5005,.F.);
#5283=ADVANCED_FACE('',(#549),#5006,.F.);
#5284=ADVANCED_FACE('',(#550),#5007,.F.);
#5285=ADVANCED_FACE('',(#551),#145,.T.);
#5286=ADVANCED_FACE('',(#552),#146,.F.);
#5287=ADVANCED_FACE('',(#553),#147,.F.);
#5288=ADVANCED_FACE('',(#554,#217),#267,.F.);
#5289=ADVANCED_FACE('',(#555,#218),#268,.F.);
#5290=ADVANCED_FACE('',(#556),#269,.T.);
#5291=ADVANCED_FACE('',(#557),#270,.T.);
#5292=ADVANCED_FACE('',(#558),#271,.T.);
#5293=ADVANCED_FACE('',(#559),#272,.T.);
#5294=ADVANCED_FACE('',(#560),#273,.T.);
#5295=ADVANCED_FACE('',(#561),#274,.T.);
#5296=ADVANCED_FACE('',(#562),#5008,.F.);
#5297=ADVANCED_FACE('',(#563),#75,.T.);
#5298=ADVANCED_FACE('',(#564),#76,.T.);
#5299=CLOSED_SHELL('',(#5009,#5010,#5011,#5012,#5013,#5014,#5015,#5016,
#5017,#5018,#5019,#5020,#5021,#5022,#5023,#5024,#5025,#5026,#5027));
#5300=CLOSED_SHELL('',(#5028,#5029,#5030,#5031,#5032,#5033,#5034,#5035,
#5036,#5037,#5038,#5039,#5040,#5041,#5042,#5043));
#5301=CLOSED_SHELL('',(#5044,#5045,#5046,#5047,#5048,#5049,#5050,#5051,
#5052,#5053,#5054,#5055,#5056,#5057,#5058,#5059,#5060,#5061,#5062,#5063,
#5064,#5065,#5066,#5067,#5068,#5069,#5070,#5071,#5072,#5073,#5074,#5075,
#5076,#5077,#5078,#5079,#5080,#5081,#5082,#5083,#5084,#5085,#5086,#5087,
#5088,#5089,#5090,#5091,#5092,#5093,#5094,#5095,#5096,#5097,#5098,#5099,
#5100,#5101,#5102,#5103,#5104,#5105,#5106,#5107,#5108,#5109,#5110,#5111,
#5112,#5113,#5114,#5115,#5116,#5117,#5118,#5119,#5120,#5121,#5122,#5123,
#5124,#5125,#5126,#5127,#5128,#5129,#5130,#5131,#5132,#5133,#5134,#5135,
#5136,#5137,#5138,#5139,#5140,#5141,#5142,#5143,#5144,#5145,#5146,#5147,
#5148,#5149,#5150,#5151,#5152,#5153,#5154,#5155,#5156,#5157,#5158,#5159,
#5160,#5161,#5162,#5163,#5164,#5165,#5166,#5167,#5168,#5169,#5170,#5171,
#5172,#5173,#5174,#5175,#5176,#5177,#5178,#5179,#5180,#5181,#5182,#5183,
#5184,#5185,#5186,#5187,#5188,#5189,#5190,#5191,#5192,#5193,#5194,#5195,
#5196,#5197,#5198,#5199,#5200,#5201,#5202,#5203,#5204,#5205,#5206,#5207,
#5208,#5209,#5210,#5211,#5212,#5213,#5214,#5215,#5216,#5217,#5218,#5219,
#5220,#5221,#5222,#5223,#5224,#5225,#5226,#5227,#5228,#5229));
#5302=CLOSED_SHELL('',(#5230,#5231,#5232,#5233,#5234,#5235,#5236,#5237,
#5238,#5239,#5240,#5241,#5242,#5243,#5244,#5245,#5246,#5247,#5248,#5249,
#5250));
#5303=CLOSED_SHELL('',(#5251,#5252,#5253,#5254,#5255,#5256,#5257,#5258,
#5259,#5260));
#5304=CLOSED_SHELL('',(#5261,#5262,#5263,#5264));
#5305=CLOSED_SHELL('',(#5265,#5266,#5267,#5268,#5269,#5270,#5271,#5272,
#5273,#5274));
#5306=CLOSED_SHELL('',(#5275,#5276,#5277,#5278,#5279,#5280,#5281,#5282,
#5283,#5284,#5285,#5286,#5287,#5288,#5289,#5290,#5291,#5292,#5293,#5294,
#5295,#5296,#5297,#5298));
#5307=DERIVED_UNIT_ELEMENT(#5323,1.);
#5308=DERIVED_UNIT_ELEMENT(#10415,-3.);
#5309=DERIVED_UNIT_ELEMENT(#5323,1.);
#5310=DERIVED_UNIT_ELEMENT(#10415,-3.);
#5311=DERIVED_UNIT_ELEMENT(#5323,1.);
#5312=DERIVED_UNIT_ELEMENT(#10415,-3.);
#5313=DERIVED_UNIT_ELEMENT(#5323,1.);
#5314=DERIVED_UNIT_ELEMENT(#10415,-3.);
#5315=DERIVED_UNIT_ELEMENT(#5323,1.);
#5316=DERIVED_UNIT_ELEMENT(#10415,-3.);
#5317=DERIVED_UNIT_ELEMENT(#5323,1.);
#5318=DERIVED_UNIT_ELEMENT(#10415,-3.);
#5319=DERIVED_UNIT_ELEMENT(#5323,1.);
#5320=DERIVED_UNIT_ELEMENT(#10415,-3.);
#5321=DERIVED_UNIT_ELEMENT(#5323,1.);
#5322=DERIVED_UNIT_ELEMENT(#10415,-3.);
#5323=(
MASS_UNIT()
NAMED_UNIT(*)
SI_UNIT(.KILO.,.GRAM.)
);
#5324=DERIVED_UNIT((#5307,#5308));
#5325=DERIVED_UNIT((#5309,#5310));
#5326=DERIVED_UNIT((#5311,#5312));
#5327=DERIVED_UNIT((#5313,#5314));
#5328=DERIVED_UNIT((#5315,#5316));
#5329=DERIVED_UNIT((#5317,#5318));
#5330=DERIVED_UNIT((#5319,#5320));
#5331=DERIVED_UNIT((#5321,#5322));
#5332=MEASURE_REPRESENTATION_ITEM('density measure',
POSITIVE_RATIO_MEASURE(7850.),#5324);
#5333=MEASURE_REPRESENTATION_ITEM('density measure',
POSITIVE_RATIO_MEASURE(7850.),#5325);
#5334=MEASURE_REPRESENTATION_ITEM('density measure',
POSITIVE_RATIO_MEASURE(7850.),#5326);
#5335=MEASURE_REPRESENTATION_ITEM('density measure',
POSITIVE_RATIO_MEASURE(7850.),#5327);
#5336=MEASURE_REPRESENTATION_ITEM('density measure',
POSITIVE_RATIO_MEASURE(7850.),#5328);
#5337=MEASURE_REPRESENTATION_ITEM('density measure',
POSITIVE_RATIO_MEASURE(7850.),#5329);
#5338=MEASURE_REPRESENTATION_ITEM('density measure',
POSITIVE_RATIO_MEASURE(7850.),#5330);
#5339=MEASURE_REPRESENTATION_ITEM('density measure',
POSITIVE_RATIO_MEASURE(7850.),#5331);
#5340=PROPERTY_DEFINITION_REPRESENTATION(#5380,#5356);
#5341=PROPERTY_DEFINITION_REPRESENTATION(#5381,#5357);
#5342=PROPERTY_DEFINITION_REPRESENTATION(#5382,#5358);
#5343=PROPERTY_DEFINITION_REPRESENTATION(#5383,#5359);
#5344=PROPERTY_DEFINITION_REPRESENTATION(#5384,#5360);
#5345=PROPERTY_DEFINITION_REPRESENTATION(#5385,#5361);
#5346=PROPERTY_DEFINITION_REPRESENTATION(#5386,#5362);
#5347=PROPERTY_DEFINITION_REPRESENTATION(#5387,#5363);
#5348=PROPERTY_DEFINITION_REPRESENTATION(#5388,#5364);
#5349=PROPERTY_DEFINITION_REPRESENTATION(#5389,#5365);
#5350=PROPERTY_DEFINITION_REPRESENTATION(#5390,#5366);
#5351=PROPERTY_DEFINITION_REPRESENTATION(#5391,#5367);
#5352=PROPERTY_DEFINITION_REPRESENTATION(#5392,#5368);
#5353=PROPERTY_DEFINITION_REPRESENTATION(#5393,#5369);
#5354=PROPERTY_DEFINITION_REPRESENTATION(#5394,#5370);
#5355=PROPERTY_DEFINITION_REPRESENTATION(#5395,#5371);
#5356=REPRESENTATION('material name',(#5372),#10405);
#5357=REPRESENTATION('density',(#5332),#10405);
#5358=REPRESENTATION('material name',(#5373),#10406);
#5359=REPRESENTATION('density',(#5333),#10406);
#5360=REPRESENTATION('material name',(#5374),#10407);
#5361=REPRESENTATION('density',(#5334),#10407);
#5362=REPRESENTATION('material name',(#5375),#10408);
#5363=REPRESENTATION('density',(#5335),#10408);
#5364=REPRESENTATION('material name',(#5376),#10409);
#5365=REPRESENTATION('density',(#5336),#10409);
#5366=REPRESENTATION('material name',(#5377),#10410);
#5367=REPRESENTATION('density',(#5337),#10410);
#5368=REPRESENTATION('material name',(#5378),#10411);
#5369=REPRESENTATION('density',(#5338),#10411);
#5370=REPRESENTATION('material name',(#5379),#10412);
#5371=REPRESENTATION('density',(#5339),#10412);
#5372=DESCRIPTIVE_REPRESENTATION_ITEM('Steel','Steel');
#5373=DESCRIPTIVE_REPRESENTATION_ITEM('Steel','Steel');
#5374=DESCRIPTIVE_REPRESENTATION_ITEM('Steel','Steel');
#5375=DESCRIPTIVE_REPRESENTATION_ITEM('Steel','Steel');
#5376=DESCRIPTIVE_REPRESENTATION_ITEM('Steel','Steel');
#5377=DESCRIPTIVE_REPRESENTATION_ITEM('Steel','Steel');
#5378=DESCRIPTIVE_REPRESENTATION_ITEM('Steel','Steel');
#5379=DESCRIPTIVE_REPRESENTATION_ITEM('Steel','Steel');
#5380=PROPERTY_DEFINITION('material property','material name',#10463);
#5381=PROPERTY_DEFINITION('material property','density of part',#10463);
#5382=PROPERTY_DEFINITION('material property','material name',#10464);
#5383=PROPERTY_DEFINITION('material property','density of part',#10464);
#5384=PROPERTY_DEFINITION('material property','material name',#10465);
#5385=PROPERTY_DEFINITION('material property','density of part',#10465);
#5386=PROPERTY_DEFINITION('material property','material name',#10466);
#5387=PROPERTY_DEFINITION('material property','density of part',#10466);
#5388=PROPERTY_DEFINITION('material property','material name',#10467);
#5389=PROPERTY_DEFINITION('material property','density of part',#10467);
#5390=PROPERTY_DEFINITION('material property','material name',#10468);
#5391=PROPERTY_DEFINITION('material property','density of part',#10468);
#5392=PROPERTY_DEFINITION('material property','material name',#10469);
#5393=PROPERTY_DEFINITION('material property','density of part',#10469);
#5394=PROPERTY_DEFINITION('material property','material name',#10470);
#5395=PROPERTY_DEFINITION('material property','density of part',#10470);
#5396=AXIS2_PLACEMENT_3D('',#7949,#6150,#6151);
#5397=AXIS2_PLACEMENT_3D('',#7950,#6152,#6153);
#5398=AXIS2_PLACEMENT_3D('',#7951,#6154,#6155);
#5399=AXIS2_PLACEMENT_3D('',#7953,#6156,#6157);
#5400=AXIS2_PLACEMENT_3D('',#7956,#6159,#6160);
#5401=AXIS2_PLACEMENT_3D('',#7957,#6161,#6162);
#5402=AXIS2_PLACEMENT_3D('',#7959,#6163,#6164);
#5403=AXIS2_PLACEMENT_3D('',#7962,#6166,#6167);
#5404=AXIS2_PLACEMENT_3D('',#7963,#6168,#6169);
#5405=AXIS2_PLACEMENT_3D('',#7965,#6170,#6171);
#5406=AXIS2_PLACEMENT_3D('',#7968,#6173,#6174);
#5407=AXIS2_PLACEMENT_3D('',#7969,#6175,#6176);
#5408=AXIS2_PLACEMENT_3D('',#7971,#6177,#6178);
#5409=AXIS2_PLACEMENT_3D('',#7974,#6180,#6181);
#5410=AXIS2_PLACEMENT_3D('',#7975,#6182,#6183);
#5411=AXIS2_PLACEMENT_3D('',#7977,#6184,#6185);
#5412=AXIS2_PLACEMENT_3D('',#7980,#6187,#6188);
#5413=AXIS2_PLACEMENT_3D('',#7981,#6189,#6190);
#5414=AXIS2_PLACEMENT_3D('',#7983,#6191,#6192);
#5415=AXIS2_PLACEMENT_3D('',#7986,#6194,#6195);
#5416=AXIS2_PLACEMENT_3D('',#7987,#6196,#6197);
#5417=AXIS2_PLACEMENT_3D('',#7989,#6198,#6199);
#5418=AXIS2_PLACEMENT_3D('',#7992,#6201,#6202);
#5419=AXIS2_PLACEMENT_3D('',#7993,#6203,#6204);
#5420=AXIS2_PLACEMENT_3D('',#7995,#6205,#6206);
#5421=AXIS2_PLACEMENT_3D('',#7998,#6208,#6209);
#5422=AXIS2_PLACEMENT_3D('',#7999,#6210,#6211);
#5423=AXIS2_PLACEMENT_3D('',#8001,#6212,#6213);
#5424=AXIS2_PLACEMENT_3D('',#8004,#6215,#6216);
#5425=AXIS2_PLACEMENT_3D('',#8005,#6217,#6218);
#5426=AXIS2_PLACEMENT_3D('',#8014,#6223,#6224);
#5427=AXIS2_PLACEMENT_3D('',#8023,#6229,#6230);
#5428=AXIS2_PLACEMENT_3D('',#8030,#6235,#6236);
#5429=AXIS2_PLACEMENT_3D('',#8037,#6241,#6242);
#5430=AXIS2_PLACEMENT_3D('',#8038,#6243,#6244);
#5431=AXIS2_PLACEMENT_3D('',#8039,#6245,#6246);
#5432=AXIS2_PLACEMENT_3D('',#8040,#6247,#6248);
#5433=AXIS2_PLACEMENT_3D('',#8042,#6250,#6251);
#5434=AXIS2_PLACEMENT_3D('',#8044,#6253,#6254);
#5435=AXIS2_PLACEMENT_3D('',#8045,#6255,#6256);
#5436=AXIS2_PLACEMENT_3D('',#8046,#6257,#6258);
#5437=AXIS2_PLACEMENT_3D('',#8048,#6259,#6260);
#5438=AXIS2_PLACEMENT_3D('',#8051,#6262,#6263);
#5439=AXIS2_PLACEMENT_3D('',#8052,#6264,#6265);
#5440=AXIS2_PLACEMENT_3D('',#8055,#6266,#6267);
#5441=AXIS2_PLACEMENT_3D('',#8059,#6269,#6270);
#5442=AXIS2_PLACEMENT_3D('',#8062,#6272,#6273);
#5443=AXIS2_PLACEMENT_3D('',#8064,#6274,#6275);
#5444=AXIS2_PLACEMENT_3D('',#8066,#6277,#6278);
#5445=AXIS2_PLACEMENT_3D('',#8068,#6279,#6280);
#5446=AXIS2_PLACEMENT_3D('',#8072,#6282,#6283);
#5447=AXIS2_PLACEMENT_3D('',#8074,#6284,#6285);
#5448=AXIS2_PLACEMENT_3D('',#8075,#6286,#6287);
#5449=AXIS2_PLACEMENT_3D('',#8076,#6288,#6289);
#5450=AXIS2_PLACEMENT_3D('',#8078,#6290,#6291);
#5451=AXIS2_PLACEMENT_3D('',#8081,#6293,#6294);
#5452=AXIS2_PLACEMENT_3D('',#8082,#6295,#6296);
#5453=AXIS2_PLACEMENT_3D('',#8084,#6297,#6298);
#5454=AXIS2_PLACEMENT_3D('',#8087,#6300,#6301);
#5455=AXIS2_PLACEMENT_3D('',#8088,#6302,#6303);
#5456=AXIS2_PLACEMENT_3D('',#8089,#6304,#6305);
#5457=AXIS2_PLACEMENT_3D('',#8090,#6306,#6307);
#5458=AXIS2_PLACEMENT_3D('',#8091,#6308,#6309);
#5459=AXIS2_PLACEMENT_3D('',#8092,#6310,#6311);
#5460=AXIS2_PLACEMENT_3D('',#8095,#6314,#6315);
#5461=AXIS2_PLACEMENT_3D('',#8101,#6319,#6320);
#5462=AXIS2_PLACEMENT_3D('',#8105,#6323,#6324);
#5463=AXIS2_PLACEMENT_3D('',#8109,#6327,#6328);
#5464=AXIS2_PLACEMENT_3D('',#8111,#6330,#6331);
#5465=AXIS2_PLACEMENT_3D('',#8112,#6332,#6333);
#5466=AXIS2_PLACEMENT_3D('',#8113,#6334,#6335);
#5467=AXIS2_PLACEMENT_3D('',#8114,#6336,#6337);
#5468=AXIS2_PLACEMENT_3D('',#8117,#6338,#6339);
#5469=AXIS2_PLACEMENT_3D('',#8121,#6341,#6342);
#5470=AXIS2_PLACEMENT_3D('',#8123,#6344,#6345);
#5471=AXIS2_PLACEMENT_3D('',#8126,#6346,#6347);
#5472=AXIS2_PLACEMENT_3D('',#8130,#6349,#6350);
#5473=AXIS2_PLACEMENT_3D('',#8132,#6352,#6353);
#5474=AXIS2_PLACEMENT_3D('',#8134,#6354,#6355);
#5475=AXIS2_PLACEMENT_3D('',#8137,#6357,#6358);
#5476=AXIS2_PLACEMENT_3D('',#8138,#6359,#6360);
#5477=AXIS2_PLACEMENT_3D('',#8141,#6361,#6362);
#5478=AXIS2_PLACEMENT_3D('',#8145,#6364,#6365);
#5479=AXIS2_PLACEMENT_3D('',#8147,#6367,#6368);
#5480=AXIS2_PLACEMENT_3D('',#8149,#6369,#6370);
#5481=AXIS2_PLACEMENT_3D('',#8152,#6372,#6373);
#5482=AXIS2_PLACEMENT_3D('',#8153,#6374,#6375);
#5483=AXIS2_PLACEMENT_3D('',#8156,#6376,#6377);
#5484=AXIS2_PLACEMENT_3D('',#8160,#6379,#6380);
#5485=AXIS2_PLACEMENT_3D('',#8162,#6382,#6383);
#5486=AXIS2_PLACEMENT_3D('',#8164,#6384,#6385);
#5487=AXIS2_PLACEMENT_3D('',#8166,#6386,#6387);
#5488=AXIS2_PLACEMENT_3D('',#8168,#6389,#6390);
#5489=AXIS2_PLACEMENT_3D('',#8171,#6391,#6392);
#5490=AXIS2_PLACEMENT_3D('',#8175,#6394,#6395);
#5491=AXIS2_PLACEMENT_3D('',#8177,#6397,#6398);
#5492=AXIS2_PLACEMENT_3D('',#8179,#6399,#6400);
#5493=AXIS2_PLACEMENT_3D('',#8181,#6401,#6402);
#5494=AXIS2_PLACEMENT_3D('',#8183,#6404,#6405);
#5495=AXIS2_PLACEMENT_3D('',#8186,#6406,#6407);
#5496=AXIS2_PLACEMENT_3D('',#8190,#6409,#6410);
#5497=AXIS2_PLACEMENT_3D('',#8192,#6412,#6413);
#5498=AXIS2_PLACEMENT_3D('',#8195,#6414,#6415);
#5499=AXIS2_PLACEMENT_3D('',#8199,#6417,#6418);
#5500=AXIS2_PLACEMENT_3D('',#8201,#6420,#6421);
#5501=AXIS2_PLACEMENT_3D('',#8204,#6422,#6423);
#5502=AXIS2_PLACEMENT_3D('',#8208,#6425,#6426);
#5503=AXIS2_PLACEMENT_3D('',#8210,#6428,#6429);
#5504=AXIS2_PLACEMENT_3D('',#8213,#6430,#6431);
#5505=AXIS2_PLACEMENT_3D('',#8217,#6433,#6434);
#5506=AXIS2_PLACEMENT_3D('',#8219,#6436,#6437);
#5507=AXIS2_PLACEMENT_3D('',#8222,#6438,#6439);
#5508=AXIS2_PLACEMENT_3D('',#8226,#6441,#6442);
#5509=AXIS2_PLACEMENT_3D('',#8228,#6444,#6445);
#5510=AXIS2_PLACEMENT_3D('',#8231,#6446,#6447);
#5511=AXIS2_PLACEMENT_3D('',#8235,#6449,#6450);
#5512=AXIS2_PLACEMENT_3D('',#8237,#6452,#6453);
#5513=AXIS2_PLACEMENT_3D('',#8240,#6454,#6455);
#5514=AXIS2_PLACEMENT_3D('',#8244,#6457,#6458);
#5515=AXIS2_PLACEMENT_3D('',#8246,#6460,#6461);
#5516=AXIS2_PLACEMENT_3D('',#8249,#6462,#6463);
#5517=AXIS2_PLACEMENT_3D('',#8253,#6465,#6466);
#5518=AXIS2_PLACEMENT_3D('',#8255,#6468,#6469);
#5519=AXIS2_PLACEMENT_3D('',#8258,#6470,#6471);
#5520=AXIS2_PLACEMENT_3D('',#8262,#6473,#6474);
#5521=AXIS2_PLACEMENT_3D('',#8264,#6476,#6477);
#5522=AXIS2_PLACEMENT_3D('',#8267,#6478,#6479);
#5523=AXIS2_PLACEMENT_3D('',#8271,#6481,#6482);
#5524=AXIS2_PLACEMENT_3D('',#8273,#6484,#6485);
#5525=AXIS2_PLACEMENT_3D('',#8276,#6486,#6487);
#5526=AXIS2_PLACEMENT_3D('',#8280,#6489,#6490);
#5527=AXIS2_PLACEMENT_3D('',#8282,#6492,#6493);
#5528=AXIS2_PLACEMENT_3D('',#8285,#6494,#6495);
#5529=AXIS2_PLACEMENT_3D('',#8289,#6497,#6498);
#5530=AXIS2_PLACEMENT_3D('',#8291,#6500,#6501);
#5531=AXIS2_PLACEMENT_3D('',#8294,#6502,#6503);
#5532=AXIS2_PLACEMENT_3D('',#8298,#6505,#6506);
#5533=AXIS2_PLACEMENT_3D('',#8300,#6508,#6509);
#5534=AXIS2_PLACEMENT_3D('',#8303,#6510,#6511);
#5535=AXIS2_PLACEMENT_3D('',#8307,#6513,#6514);
#5536=AXIS2_PLACEMENT_3D('',#8309,#6516,#6517);
#5537=AXIS2_PLACEMENT_3D('',#8312,#6518,#6519);
#5538=AXIS2_PLACEMENT_3D('',#8316,#6521,#6522);
#5539=AXIS2_PLACEMENT_3D('',#8318,#6524,#6525);
#5540=AXIS2_PLACEMENT_3D('',#8321,#6526,#6527);
#5541=AXIS2_PLACEMENT_3D('',#8325,#6529,#6530);
#5542=AXIS2_PLACEMENT_3D('',#8327,#6532,#6533);
#5543=AXIS2_PLACEMENT_3D('',#8330,#6534,#6535);
#5544=AXIS2_PLACEMENT_3D('',#8334,#6537,#6538);
#5545=AXIS2_PLACEMENT_3D('',#8336,#6540,#6541);
#5546=AXIS2_PLACEMENT_3D('',#8339,#6542,#6543);
#5547=AXIS2_PLACEMENT_3D('',#8343,#6545,#6546);
#5548=AXIS2_PLACEMENT_3D('',#8345,#6548,#6549);
#5549=AXIS2_PLACEMENT_3D('',#8348,#6550,#6551);
#5550=AXIS2_PLACEMENT_3D('',#8352,#6553,#6554);
#5551=AXIS2_PLACEMENT_3D('',#8354,#6556,#6557);
#5552=AXIS2_PLACEMENT_3D('',#8357,#6558,#6559);
#5553=AXIS2_PLACEMENT_3D('',#8361,#6561,#6562);
#5554=AXIS2_PLACEMENT_3D('',#8363,#6564,#6565);
#5555=AXIS2_PLACEMENT_3D('',#8366,#6566,#6567);
#5556=AXIS2_PLACEMENT_3D('',#8370,#6569,#6570);
#5557=AXIS2_PLACEMENT_3D('',#8372,#6572,#6573);
#5558=AXIS2_PLACEMENT_3D('',#8375,#6574,#6575);
#5559=AXIS2_PLACEMENT_3D('',#8379,#6577,#6578);
#5560=AXIS2_PLACEMENT_3D('',#8381,#6580,#6581);
#5561=AXIS2_PLACEMENT_3D('',#8384,#6582,#6583);
#5562=AXIS2_PLACEMENT_3D('',#8388,#6585,#6586);
#5563=AXIS2_PLACEMENT_3D('',#8390,#6588,#6589);
#5564=AXIS2_PLACEMENT_3D('',#8393,#6590,#6591);
#5565=AXIS2_PLACEMENT_3D('',#8397,#6593,#6594);
#5566=AXIS2_PLACEMENT_3D('',#8399,#6596,#6597);
#5567=AXIS2_PLACEMENT_3D('',#8401,#6598,#6599);
#5568=AXIS2_PLACEMENT_3D('',#8404,#6601,#6602);
#5569=AXIS2_PLACEMENT_3D('',#8405,#6603,#6604);
#5570=AXIS2_PLACEMENT_3D('',#8407,#6605,#6606);
#5571=AXIS2_PLACEMENT_3D('',#8410,#6608,#6609);
#5572=AXIS2_PLACEMENT_3D('',#8411,#6610,#6611);
#5573=AXIS2_PLACEMENT_3D('',#8413,#6612,#6613);
#5574=AXIS2_PLACEMENT_3D('',#8416,#6615,#6616);
#5575=AXIS2_PLACEMENT_3D('',#8417,#6617,#6618);
#5576=AXIS2_PLACEMENT_3D('',#8420,#6619,#6620);
#5577=AXIS2_PLACEMENT_3D('',#8424,#6622,#6623);
#5578=AXIS2_PLACEMENT_3D('',#8426,#6625,#6626);
#5579=AXIS2_PLACEMENT_3D('',#8429,#6627,#6628);
#5580=AXIS2_PLACEMENT_3D('',#8433,#6630,#6631);
#5581=AXIS2_PLACEMENT_3D('',#8435,#6633,#6634);
#5582=AXIS2_PLACEMENT_3D('',#8438,#6635,#6636);
#5583=AXIS2_PLACEMENT_3D('',#8442,#6638,#6639);
#5584=AXIS2_PLACEMENT_3D('',#8444,#6641,#6642);
#5585=AXIS2_PLACEMENT_3D('',#8447,#6643,#6644);
#5586=AXIS2_PLACEMENT_3D('',#8451,#6646,#6647);
#5587=AXIS2_PLACEMENT_3D('',#8453,#6649,#6650);
#5588=AXIS2_PLACEMENT_3D('',#8456,#6651,#6652);
#5589=AXIS2_PLACEMENT_3D('',#8460,#6654,#6655);
#5590=AXIS2_PLACEMENT_3D('',#8462,#6657,#6658);
#5591=AXIS2_PLACEMENT_3D('',#8465,#6659,#6660);
#5592=AXIS2_PLACEMENT_3D('',#8469,#6662,#6663);
#5593=AXIS2_PLACEMENT_3D('',#8471,#6665,#6666);
#5594=AXIS2_PLACEMENT_3D('',#8474,#6667,#6668);
#5595=AXIS2_PLACEMENT_3D('',#8478,#6670,#6671);
#5596=AXIS2_PLACEMENT_3D('',#8480,#6673,#6674);
#5597=AXIS2_PLACEMENT_3D('',#8483,#6675,#6676);
#5598=AXIS2_PLACEMENT_3D('',#8487,#6678,#6679);
#5599=AXIS2_PLACEMENT_3D('',#8489,#6681,#6682);
#5600=AXIS2_PLACEMENT_3D('',#8492,#6683,#6684);
#5601=AXIS2_PLACEMENT_3D('',#8496,#6686,#6687);
#5602=AXIS2_PLACEMENT_3D('',#8498,#6689,#6690);
#5603=AXIS2_PLACEMENT_3D('',#8501,#6691,#6692);
#5604=AXIS2_PLACEMENT_3D('',#8505,#6694,#6695);
#5605=AXIS2_PLACEMENT_3D('',#8507,#6697,#6698);
#5606=AXIS2_PLACEMENT_3D('',#8510,#6699,#6700);
#5607=AXIS2_PLACEMENT_3D('',#8514,#6702,#6703);
#5608=AXIS2_PLACEMENT_3D('',#8516,#6705,#6706);
#5609=AXIS2_PLACEMENT_3D('',#8519,#6707,#6708);
#5610=AXIS2_PLACEMENT_3D('',#8523,#6710,#6711);
#5611=AXIS2_PLACEMENT_3D('',#8525,#6713,#6714);
#5612=AXIS2_PLACEMENT_3D('',#8527,#6715,#6716);
#5613=AXIS2_PLACEMENT_3D('',#8529,#6717,#6718);
#5614=AXIS2_PLACEMENT_3D('',#8531,#6719,#6720);
#5615=AXIS2_PLACEMENT_3D('',#8533,#6721,#6722);
#5616=AXIS2_PLACEMENT_3D('',#8534,#6723,#6724);
#5617=AXIS2_PLACEMENT_3D('',#8536,#6725,#6726);
#5618=AXIS2_PLACEMENT_3D('',#8538,#6727,#6728);
#5619=AXIS2_PLACEMENT_3D('',#8540,#6729,#6730);
#5620=AXIS2_PLACEMENT_3D('',#8542,#6731,#6732);
#5621=AXIS2_PLACEMENT_3D('',#8543,#6733,#6734);
#5622=AXIS2_PLACEMENT_3D('',#8545,#6735,#6736);
#5623=AXIS2_PLACEMENT_3D('',#8547,#6737,#6738);
#5624=AXIS2_PLACEMENT_3D('',#8549,#6739,#6740);
#5625=AXIS2_PLACEMENT_3D('',#8551,#6741,#6742);
#5626=AXIS2_PLACEMENT_3D('',#8552,#6743,#6744);
#5627=AXIS2_PLACEMENT_3D('',#8554,#6745,#6746);
#5628=AXIS2_PLACEMENT_3D('',#8556,#6747,#6748);
#5629=AXIS2_PLACEMENT_3D('',#8558,#6749,#6750);
#5630=AXIS2_PLACEMENT_3D('',#8560,#6751,#6752);
#5631=AXIS2_PLACEMENT_3D('',#8561,#6753,#6754);
#5632=AXIS2_PLACEMENT_3D('',#8563,#6755,#6756);
#5633=AXIS2_PLACEMENT_3D('',#8565,#6757,#6758);
#5634=AXIS2_PLACEMENT_3D('',#8567,#6759,#6760);
#5635=AXIS2_PLACEMENT_3D('',#8569,#6761,#6762);
#5636=AXIS2_PLACEMENT_3D('',#8570,#6763,#6764);
#5637=AXIS2_PLACEMENT_3D('',#8572,#6765,#6766);
#5638=AXIS2_PLACEMENT_3D('',#8574,#6767,#6768);
#5639=AXIS2_PLACEMENT_3D('',#8576,#6769,#6770);
#5640=AXIS2_PLACEMENT_3D('',#8578,#6771,#6772);
#5641=AXIS2_PLACEMENT_3D('',#8579,#6773,#6774);
#5642=AXIS2_PLACEMENT_3D('',#8581,#6775,#6776);
#5643=AXIS2_PLACEMENT_3D('',#8583,#6777,#6778);
#5644=AXIS2_PLACEMENT_3D('',#8585,#6779,#6780);
#5645=AXIS2_PLACEMENT_3D('',#8587,#6781,#6782);
#5646=AXIS2_PLACEMENT_3D('',#8588,#6783,#6784);
#5647=AXIS2_PLACEMENT_3D('',#8590,#6785,#6786);
#5648=AXIS2_PLACEMENT_3D('',#8592,#6787,#6788);
#5649=AXIS2_PLACEMENT_3D('',#8594,#6789,#6790);
#5650=AXIS2_PLACEMENT_3D('',#8596,#6791,#6792);
#5651=AXIS2_PLACEMENT_3D('',#8597,#6793,#6794);
#5652=AXIS2_PLACEMENT_3D('',#8599,#6795,#6796);
#5653=AXIS2_PLACEMENT_3D('',#8601,#6797,#6798);
#5654=AXIS2_PLACEMENT_3D('',#8603,#6799,#6800);
#5655=AXIS2_PLACEMENT_3D('',#8605,#6801,#6802);
#5656=AXIS2_PLACEMENT_3D('',#8606,#6803,#6804);
#5657=AXIS2_PLACEMENT_3D('',#8608,#6805,#6806);
#5658=AXIS2_PLACEMENT_3D('',#8610,#6807,#6808);
#5659=AXIS2_PLACEMENT_3D('',#8612,#6809,#6810);
#5660=AXIS2_PLACEMENT_3D('',#8614,#6811,#6812);
#5661=AXIS2_PLACEMENT_3D('',#8615,#6813,#6814);
#5662=AXIS2_PLACEMENT_3D('',#8617,#6815,#6816);
#5663=AXIS2_PLACEMENT_3D('',#8619,#6817,#6818);
#5664=AXIS2_PLACEMENT_3D('',#8621,#6819,#6820);
#5665=AXIS2_PLACEMENT_3D('',#8623,#6821,#6822);
#5666=AXIS2_PLACEMENT_3D('',#8624,#6823,#6824);
#5667=AXIS2_PLACEMENT_3D('',#8626,#6825,#6826);
#5668=AXIS2_PLACEMENT_3D('',#8628,#6827,#6828);
#5669=AXIS2_PLACEMENT_3D('',#8630,#6829,#6830);
#5670=AXIS2_PLACEMENT_3D('',#8632,#6831,#6832);
#5671=AXIS2_PLACEMENT_3D('',#8633,#6833,#6834);
#5672=AXIS2_PLACEMENT_3D('',#8635,#6835,#6836);
#5673=AXIS2_PLACEMENT_3D('',#8637,#6837,#6838);
#5674=AXIS2_PLACEMENT_3D('',#8638,#6839,#6840);
#5675=AXIS2_PLACEMENT_3D('',#8640,#6841,#6842);
#5676=AXIS2_PLACEMENT_3D('',#8642,#6843,#6844);
#5677=AXIS2_PLACEMENT_3D('',#8643,#6845,#6846);
#5678=AXIS2_PLACEMENT_3D('',#8644,#6847,#6848);
#5679=AXIS2_PLACEMENT_3D('',#8646,#6849,#6850);
#5680=AXIS2_PLACEMENT_3D('',#8648,#6851,#6852);
#5681=AXIS2_PLACEMENT_3D('',#8649,#6853,#6854);
#5682=AXIS2_PLACEMENT_3D('',#8650,#6855,#6856);
#5683=AXIS2_PLACEMENT_3D('',#8652,#6857,#6858);
#5684=AXIS2_PLACEMENT_3D('',#8654,#6859,#6860);
#5685=AXIS2_PLACEMENT_3D('',#8655,#6861,#6862);
#5686=AXIS2_PLACEMENT_3D('',#8656,#6863,#6864);
#5687=AXIS2_PLACEMENT_3D('',#8658,#6865,#6866);
#5688=AXIS2_PLACEMENT_3D('',#8660,#6867,#6868);
#5689=AXIS2_PLACEMENT_3D('',#8661,#6869,#6870);
#5690=AXIS2_PLACEMENT_3D('',#8662,#6871,#6872);
#5691=AXIS2_PLACEMENT_3D('',#8664,#6873,#6874);
#5692=AXIS2_PLACEMENT_3D('',#8666,#6875,#6876);
#5693=AXIS2_PLACEMENT_3D('',#8667,#6877,#6878);
#5694=AXIS2_PLACEMENT_3D('',#8668,#6879,#6880);
#5695=AXIS2_PLACEMENT_3D('',#8670,#6881,#6882);
#5696=AXIS2_PLACEMENT_3D('',#8672,#6883,#6884);
#5697=AXIS2_PLACEMENT_3D('',#8673,#6885,#6886);
#5698=AXIS2_PLACEMENT_3D('',#8675,#6887,#6888);
#5699=AXIS2_PLACEMENT_3D('',#8677,#6889,#6890);
#5700=AXIS2_PLACEMENT_3D('',#8678,#6891,#6892);
#5701=AXIS2_PLACEMENT_3D('',#8679,#6893,#6894);
#5702=AXIS2_PLACEMENT_3D('',#8681,#6895,#6896);
#5703=AXIS2_PLACEMENT_3D('',#8683,#6897,#6898);
#5704=AXIS2_PLACEMENT_3D('',#8684,#6899,#6900);
#5705=AXIS2_PLACEMENT_3D('',#8685,#6901,#6902);
#5706=AXIS2_PLACEMENT_3D('',#8687,#6903,#6904);
#5707=AXIS2_PLACEMENT_3D('',#8689,#6905,#6906);
#5708=AXIS2_PLACEMENT_3D('',#8690,#6907,#6908);
#5709=AXIS2_PLACEMENT_3D('',#8691,#6909,#6910);
#5710=AXIS2_PLACEMENT_3D('',#8693,#6911,#6912);
#5711=AXIS2_PLACEMENT_3D('',#8695,#6913,#6914);
#5712=AXIS2_PLACEMENT_3D('',#8696,#6915,#6916);
#5713=AXIS2_PLACEMENT_3D('',#8697,#6917,#6918);
#5714=AXIS2_PLACEMENT_3D('',#8699,#6919,#6920);
#5715=AXIS2_PLACEMENT_3D('',#8701,#6921,#6922);
#5716=AXIS2_PLACEMENT_3D('',#8702,#6923,#6924);
#5717=AXIS2_PLACEMENT_3D('',#8703,#6925,#6926);
#5718=AXIS2_PLACEMENT_3D('',#8705,#6927,#6928);
#5719=AXIS2_PLACEMENT_3D('',#8707,#6929,#6930);
#5720=AXIS2_PLACEMENT_3D('',#8708,#6931,#6932);
#5721=AXIS2_PLACEMENT_3D('',#8710,#6933,#6934);
#5722=AXIS2_PLACEMENT_3D('',#8712,#6935,#6936);
#5723=AXIS2_PLACEMENT_3D('',#8713,#6937,#6938);
#5724=AXIS2_PLACEMENT_3D('',#8715,#6939,#6940);
#5725=AXIS2_PLACEMENT_3D('',#8717,#6941,#6942);
#5726=AXIS2_PLACEMENT_3D('',#8719,#6943,#6944);
#5727=AXIS2_PLACEMENT_3D('',#8721,#6945,#6946);
#5728=AXIS2_PLACEMENT_3D('',#8723,#6947,#6948);
#5729=AXIS2_PLACEMENT_3D('',#8724,#6949,#6950);
#5730=AXIS2_PLACEMENT_3D('',#8726,#6951,#6952);
#5731=AXIS2_PLACEMENT_3D('',#8728,#6953,#6954);
#5732=AXIS2_PLACEMENT_3D('',#8730,#6955,#6956);
#5733=AXIS2_PLACEMENT_3D('',#8732,#6957,#6958);
#5734=AXIS2_PLACEMENT_3D('',#8733,#6959,#6960);
#5735=AXIS2_PLACEMENT_3D('',#8735,#6961,#6962);
#5736=AXIS2_PLACEMENT_3D('',#8737,#6963,#6964);
#5737=AXIS2_PLACEMENT_3D('',#8739,#6965,#6966);
#5738=AXIS2_PLACEMENT_3D('',#8741,#6967,#6968);
#5739=AXIS2_PLACEMENT_3D('',#8742,#6969,#6970);
#5740=AXIS2_PLACEMENT_3D('',#8744,#6971,#6972);
#5741=AXIS2_PLACEMENT_3D('',#8746,#6973,#6974);
#5742=AXIS2_PLACEMENT_3D('',#8748,#6975,#6976);
#5743=AXIS2_PLACEMENT_3D('',#8750,#6977,#6978);
#5744=AXIS2_PLACEMENT_3D('',#8751,#6979,#6980);
#5745=AXIS2_PLACEMENT_3D('',#8757,#6984,#6985);
#5746=AXIS2_PLACEMENT_3D('',#8759,#6986,#6987);
#5747=AXIS2_PLACEMENT_3D('',#8761,#6988,#6989);
#5748=AXIS2_PLACEMENT_3D('',#8763,#6990,#6991);
#5749=AXIS2_PLACEMENT_3D('',#8765,#6992,#6993);
#5750=AXIS2_PLACEMENT_3D('',#8767,#6994,#6995);
#5751=AXIS2_PLACEMENT_3D('',#8768,#6996,#6997);
#5752=AXIS2_PLACEMENT_3D('',#8770,#6998,#6999);
#5753=AXIS2_PLACEMENT_3D('',#8772,#7000,#7001);
#5754=AXIS2_PLACEMENT_3D('',#8774,#7002,#7003);
#5755=AXIS2_PLACEMENT_3D('',#8776,#7004,#7005);
#5756=AXIS2_PLACEMENT_3D('',#8777,#7006,#7007);
#5757=AXIS2_PLACEMENT_3D('',#8779,#7008,#7009);
#5758=AXIS2_PLACEMENT_3D('',#8781,#7010,#7011);
#5759=AXIS2_PLACEMENT_3D('',#8783,#7012,#7013);
#5760=AXIS2_PLACEMENT_3D('',#8785,#7014,#7015);
#5761=AXIS2_PLACEMENT_3D('',#8786,#7016,#7017);
#5762=AXIS2_PLACEMENT_3D('',#8788,#7018,#7019);
#5763=AXIS2_PLACEMENT_3D('',#8790,#7020,#7021);
#5764=AXIS2_PLACEMENT_3D('',#8792,#7022,#7023);
#5765=AXIS2_PLACEMENT_3D('',#8794,#7024,#7025);
#5766=AXIS2_PLACEMENT_3D('',#8796,#7026,#7027);
#5767=AXIS2_PLACEMENT_3D('',#8797,#7028,#7029);
#5768=AXIS2_PLACEMENT_3D('',#8799,#7030,#7031);
#5769=AXIS2_PLACEMENT_3D('',#8801,#7032,#7033);
#5770=AXIS2_PLACEMENT_3D('',#8802,#7034,#7035);
#5771=AXIS2_PLACEMENT_3D('',#8804,#7036,#7037);
#5772=AXIS2_PLACEMENT_3D('',#8806,#7038,#7039);
#5773=AXIS2_PLACEMENT_3D('',#8807,#7040,#7041);
#5774=AXIS2_PLACEMENT_3D('',#8808,#7042,#7043);
#5775=AXIS2_PLACEMENT_3D('',#8810,#7044,#7045);
#5776=AXIS2_PLACEMENT_3D('',#8812,#7046,#7047);
#5777=AXIS2_PLACEMENT_3D('',#8813,#7048,#7049);
#5778=AXIS2_PLACEMENT_3D('',#8814,#7050,#7051);
#5779=AXIS2_PLACEMENT_3D('',#8816,#7052,#7053);
#5780=AXIS2_PLACEMENT_3D('',#8818,#7054,#7055);
#5781=AXIS2_PLACEMENT_3D('',#8819,#7056,#7057);
#5782=AXIS2_PLACEMENT_3D('',#8820,#7058,#7059);
#5783=AXIS2_PLACEMENT_3D('',#8822,#7060,#7061);
#5784=AXIS2_PLACEMENT_3D('',#8824,#7062,#7063);
#5785=AXIS2_PLACEMENT_3D('',#8825,#7064,#7065);
#5786=AXIS2_PLACEMENT_3D('',#8826,#7066,#7067);
#5787=AXIS2_PLACEMENT_3D('',#8828,#7068,#7069);
#5788=AXIS2_PLACEMENT_3D('',#8830,#7070,#7071);
#5789=AXIS2_PLACEMENT_3D('',#8831,#7072,#7073);
#5790=AXIS2_PLACEMENT_3D('',#8832,#7074,#7075);
#5791=AXIS2_PLACEMENT_3D('',#8834,#7076,#7077);
#5792=AXIS2_PLACEMENT_3D('',#8836,#7078,#7079);
#5793=AXIS2_PLACEMENT_3D('',#8837,#7080,#7081);
#5794=AXIS2_PLACEMENT_3D('',#8839,#7082,#7083);
#5795=AXIS2_PLACEMENT_3D('',#8841,#7084,#7085);
#5796=AXIS2_PLACEMENT_3D('',#8842,#7086,#7087);
#5797=AXIS2_PLACEMENT_3D('',#8843,#7088,#7089);
#5798=AXIS2_PLACEMENT_3D('',#8845,#7090,#7091);
#5799=AXIS2_PLACEMENT_3D('',#8847,#7092,#7093);
#5800=AXIS2_PLACEMENT_3D('',#8848,#7094,#7095);
#5801=AXIS2_PLACEMENT_3D('',#8849,#7096,#7097);
#5802=AXIS2_PLACEMENT_3D('',#8851,#7098,#7099);
#5803=AXIS2_PLACEMENT_3D('',#8853,#7100,#7101);
#5804=AXIS2_PLACEMENT_3D('',#8854,#7102,#7103);
#5805=AXIS2_PLACEMENT_3D('',#8855,#7104,#7105);
#5806=AXIS2_PLACEMENT_3D('',#8857,#7106,#7107);
#5807=AXIS2_PLACEMENT_3D('',#8859,#7108,#7109);
#5808=AXIS2_PLACEMENT_3D('',#8860,#7110,#7111);
#5809=AXIS2_PLACEMENT_3D('',#8861,#7112,#7113);
#5810=AXIS2_PLACEMENT_3D('',#8863,#7114,#7115);
#5811=AXIS2_PLACEMENT_3D('',#8865,#7116,#7117);
#5812=AXIS2_PLACEMENT_3D('',#8866,#7118,#7119);
#5813=AXIS2_PLACEMENT_3D('',#8867,#7120,#7121);
#5814=AXIS2_PLACEMENT_3D('',#8869,#7122,#7123);
#5815=AXIS2_PLACEMENT_3D('',#8871,#7124,#7125);
#5816=AXIS2_PLACEMENT_3D('',#8872,#7126,#7127);
#5817=AXIS2_PLACEMENT_3D('',#8874,#7128,#7129);
#5818=AXIS2_PLACEMENT_3D('',#8876,#7130,#7131);
#5819=AXIS2_PLACEMENT_3D('',#8877,#7132,#7133);
#5820=AXIS2_PLACEMENT_3D('',#8879,#7134,#7135);
#5821=AXIS2_PLACEMENT_3D('',#8881,#7136,#7137);
#5822=AXIS2_PLACEMENT_3D('',#8883,#7138,#7139);
#5823=AXIS2_PLACEMENT_3D('',#8885,#7140,#7141);
#5824=AXIS2_PLACEMENT_3D('',#8886,#7142,#7143);
#5825=AXIS2_PLACEMENT_3D('',#8888,#7144,#7145);
#5826=AXIS2_PLACEMENT_3D('',#8890,#7146,#7147);
#5827=AXIS2_PLACEMENT_3D('',#8892,#7148,#7149);
#5828=AXIS2_PLACEMENT_3D('',#8894,#7150,#7151);
#5829=AXIS2_PLACEMENT_3D('',#8895,#7152,#7153);
#5830=AXIS2_PLACEMENT_3D('',#8897,#7154,#7155);
#5831=AXIS2_PLACEMENT_3D('',#8899,#7156,#7157);
#5832=AXIS2_PLACEMENT_3D('',#8901,#7158,#7159);
#5833=AXIS2_PLACEMENT_3D('',#8903,#7160,#7161);
#5834=AXIS2_PLACEMENT_3D('',#8904,#7162,#7163);
#5835=AXIS2_PLACEMENT_3D('',#8906,#7164,#7165);
#5836=AXIS2_PLACEMENT_3D('',#8908,#7166,#7167);
#5837=AXIS2_PLACEMENT_3D('',#8910,#7168,#7169);
#5838=AXIS2_PLACEMENT_3D('',#8912,#7170,#7171);
#5839=AXIS2_PLACEMENT_3D('',#8913,#7172,#7173);
#5840=AXIS2_PLACEMENT_3D('',#8915,#7174,#7175);
#5841=AXIS2_PLACEMENT_3D('',#8917,#7176,#7177);
#5842=AXIS2_PLACEMENT_3D('',#8919,#7178,#7179);
#5843=AXIS2_PLACEMENT_3D('',#8921,#7180,#7181);
#5844=AXIS2_PLACEMENT_3D('',#8922,#7182,#7183);
#5845=AXIS2_PLACEMENT_3D('',#8924,#7184,#7185);
#5846=AXIS2_PLACEMENT_3D('',#8926,#7186,#7187);
#5847=AXIS2_PLACEMENT_3D('',#8928,#7188,#7189);
#5848=AXIS2_PLACEMENT_3D('',#8930,#7190,#7191);
#5849=AXIS2_PLACEMENT_3D('',#8931,#7192,#7193);
#5850=AXIS2_PLACEMENT_3D('',#8933,#7194,#7195);
#5851=AXIS2_PLACEMENT_3D('',#8935,#7196,#7197);
#5852=AXIS2_PLACEMENT_3D('',#8937,#7198,#7199);
#5853=AXIS2_PLACEMENT_3D('',#8939,#7200,#7201);
#5854=AXIS2_PLACEMENT_3D('',#8940,#7202,#7203);
#5855=AXIS2_PLACEMENT_3D('',#8942,#7204,#7205);
#5856=AXIS2_PLACEMENT_3D('',#8944,#7206,#7207);
#5857=AXIS2_PLACEMENT_3D('',#8946,#7208,#7209);
#5858=AXIS2_PLACEMENT_3D('',#8948,#7210,#7211);
#5859=AXIS2_PLACEMENT_3D('',#8949,#7212,#7213);
#5860=AXIS2_PLACEMENT_3D('',#8951,#7214,#7215);
#5861=AXIS2_PLACEMENT_3D('',#8953,#7216,#7217);
#5862=AXIS2_PLACEMENT_3D('',#8955,#7218,#7219);
#5863=AXIS2_PLACEMENT_3D('',#8957,#7220,#7221);
#5864=AXIS2_PLACEMENT_3D('',#8958,#7222,#7223);
#5865=AXIS2_PLACEMENT_3D('',#8960,#7224,#7225);
#5866=AXIS2_PLACEMENT_3D('',#8962,#7226,#7227);
#5867=AXIS2_PLACEMENT_3D('',#8964,#7228,#7229);
#5868=AXIS2_PLACEMENT_3D('',#8966,#7230,#7231);
#5869=AXIS2_PLACEMENT_3D('',#8967,#7232,#7233);
#5870=AXIS2_PLACEMENT_3D('',#8969,#7234,#7235);
#5871=AXIS2_PLACEMENT_3D('',#8971,#7236,#7237);
#5872=AXIS2_PLACEMENT_3D('',#8973,#7238,#7239);
#5873=AXIS2_PLACEMENT_3D('',#8975,#7240,#7241);
#5874=AXIS2_PLACEMENT_3D('',#8976,#7242,#7243);
#5875=AXIS2_PLACEMENT_3D('',#8978,#7244,#7245);
#5876=AXIS2_PLACEMENT_3D('',#8980,#7246,#7247);
#5877=AXIS2_PLACEMENT_3D('',#8982,#7248,#7249);
#5878=AXIS2_PLACEMENT_3D('',#8983,#7250,#7251);
#5879=AXIS2_PLACEMENT_3D('',#8989,#7255,#7256);
#5880=AXIS2_PLACEMENT_3D('',#8991,#7258,#7259);
#5881=AXIS2_PLACEMENT_3D('',#8993,#7261,#7262);
#5882=AXIS2_PLACEMENT_3D('',#8995,#7264,#7265);
#5883=AXIS2_PLACEMENT_3D('',#8998,#7268,#7269);
#5884=AXIS2_PLACEMENT_3D('',#8999,#7270,#7271);
#5885=AXIS2_PLACEMENT_3D('',#9000,#7272,#7273);
#5886=AXIS2_PLACEMENT_3D('',#9002,#7275,#7276);
#5887=AXIS2_PLACEMENT_3D('',#9004,#7278,#7279);
#5888=AXIS2_PLACEMENT_3D('',#9006,#7281,#7282);
#5889=AXIS2_PLACEMENT_3D('',#9008,#7284,#7285);
#5890=AXIS2_PLACEMENT_3D('',#9009,#7286,#7287);
#5891=AXIS2_PLACEMENT_3D('',#9010,#7288,#7289);
#5892=AXIS2_PLACEMENT_3D('',#9012,#7291,#7292);
#5893=AXIS2_PLACEMENT_3D('',#9014,#7294,#7295);
#5894=AXIS2_PLACEMENT_3D('',#9015,#7296,#7297);
#5895=AXIS2_PLACEMENT_3D('',#9016,#7298,#7299);
#5896=AXIS2_PLACEMENT_3D('',#9018,#7301,#7302);
#5897=AXIS2_PLACEMENT_3D('',#9020,#7304,#7305);
#5898=AXIS2_PLACEMENT_3D('',#9021,#7306,#7307);
#5899=AXIS2_PLACEMENT_3D('',#9022,#7308,#7309);
#5900=AXIS2_PLACEMENT_3D('',#9024,#7311,#7312);
#5901=AXIS2_PLACEMENT_3D('',#9026,#7314,#7315);
#5902=AXIS2_PLACEMENT_3D('',#9027,#7316,#7317);
#5903=AXIS2_PLACEMENT_3D('',#9028,#7318,#7319);
#5904=AXIS2_PLACEMENT_3D('',#9030,#7321,#7322);
#5905=AXIS2_PLACEMENT_3D('',#9032,#7324,#7325);
#5906=AXIS2_PLACEMENT_3D('',#9033,#7326,#7327);
#5907=AXIS2_PLACEMENT_3D('',#9034,#7328,#7329);
#5908=AXIS2_PLACEMENT_3D('',#9036,#7331,#7332);
#5909=AXIS2_PLACEMENT_3D('',#9038,#7334,#7335);
#5910=AXIS2_PLACEMENT_3D('',#9039,#7336,#7337);
#5911=AXIS2_PLACEMENT_3D('',#9041,#7339,#7340);
#5912=AXIS2_PLACEMENT_3D('',#9042,#7341,#7342);
#5913=AXIS2_PLACEMENT_3D('',#9044,#7344,#7345);
#5914=AXIS2_PLACEMENT_3D('',#9045,#7346,#7347);
#5915=AXIS2_PLACEMENT_3D('',#9047,#7349,#7350);
#5916=AXIS2_PLACEMENT_3D('',#9048,#7351,#7352);
#5917=AXIS2_PLACEMENT_3D('',#9050,#7354,#7355);
#5918=AXIS2_PLACEMENT_3D('',#9051,#7356,#7357);
#5919=AXIS2_PLACEMENT_3D('',#9053,#7359,#7360);
#5920=AXIS2_PLACEMENT_3D('',#9054,#7361,#7362);
#5921=AXIS2_PLACEMENT_3D('',#9056,#7364,#7365);
#5922=AXIS2_PLACEMENT_3D('',#9057,#7366,#7367);
#5923=AXIS2_PLACEMENT_3D('',#9059,#7369,#7370);
#5924=AXIS2_PLACEMENT_3D('',#9060,#7371,#7372);
#5925=AXIS2_PLACEMENT_3D('',#9062,#7374,#7375);
#5926=AXIS2_PLACEMENT_3D('',#9063,#7376,#7377);
#5927=AXIS2_PLACEMENT_3D('',#9065,#7379,#7380);
#5928=AXIS2_PLACEMENT_3D('',#9066,#7381,#7382);
#5929=AXIS2_PLACEMENT_3D('',#9068,#7384,#7385);
#5930=AXIS2_PLACEMENT_3D('',#9069,#7386,#7387);
#5931=AXIS2_PLACEMENT_3D('',#9071,#7389,#7390);
#5932=AXIS2_PLACEMENT_3D('',#9073,#7392,#7393);
#5933=AXIS2_PLACEMENT_3D('',#9074,#7394,#7395);
#5934=AXIS2_PLACEMENT_3D('',#9076,#7397,#7398);
#5935=AXIS2_PLACEMENT_3D('',#9078,#7400,#7401);
#5936=AXIS2_PLACEMENT_3D('',#9079,#7402,#7403);
#5937=AXIS2_PLACEMENT_3D('',#9081,#7405,#7406);
#5938=AXIS2_PLACEMENT_3D('',#9083,#7408,#7409);
#5939=AXIS2_PLACEMENT_3D('',#9084,#7410,#7411);
#5940=AXIS2_PLACEMENT_3D('',#9086,#7413,#7414);
#5941=AXIS2_PLACEMENT_3D('',#9088,#7416,#7417);
#5942=AXIS2_PLACEMENT_3D('',#9089,#7418,#7419);
#5943=AXIS2_PLACEMENT_3D('',#9091,#7421,#7422);
#5944=AXIS2_PLACEMENT_3D('',#9093,#7424,#7425);
#5945=AXIS2_PLACEMENT_3D('',#9095,#7427,#7428);
#5946=AXIS2_PLACEMENT_3D('',#9097,#7430,#7431);
#5947=AXIS2_PLACEMENT_3D('',#9098,#7432,#7433);
#5948=AXIS2_PLACEMENT_3D('',#9100,#7435,#7436);
#5949=AXIS2_PLACEMENT_3D('',#9102,#7438,#7439);
#5950=AXIS2_PLACEMENT_3D('',#9104,#7441,#7442);
#5951=AXIS2_PLACEMENT_3D('',#9106,#7444,#7445);
#5952=AXIS2_PLACEMENT_3D('',#9107,#7446,#7447);
#5953=AXIS2_PLACEMENT_3D('',#9109,#7449,#7450);
#5954=AXIS2_PLACEMENT_3D('',#9111,#7452,#7453);
#5955=AXIS2_PLACEMENT_3D('',#9113,#7455,#7456);
#5956=AXIS2_PLACEMENT_3D('',#9115,#7458,#7459);
#5957=AXIS2_PLACEMENT_3D('',#9116,#7460,#7461);
#5958=AXIS2_PLACEMENT_3D('',#9118,#7463,#7464);
#5959=AXIS2_PLACEMENT_3D('',#9120,#7466,#7467);
#5960=AXIS2_PLACEMENT_3D('',#9122,#7469,#7470);
#5961=AXIS2_PLACEMENT_3D('',#9124,#7472,#7473);
#5962=AXIS2_PLACEMENT_3D('',#9125,#7474,#7475);
#5963=AXIS2_PLACEMENT_3D('',#9127,#7477,#7478);
#5964=AXIS2_PLACEMENT_3D('',#9129,#7480,#7481);
#5965=AXIS2_PLACEMENT_3D('',#9131,#7483,#7484);
#5966=AXIS2_PLACEMENT_3D('',#9133,#7486,#7487);
#5967=AXIS2_PLACEMENT_3D('',#9134,#7488,#7489);
#5968=AXIS2_PLACEMENT_3D('',#9136,#7491,#7492);
#5969=AXIS2_PLACEMENT_3D('',#9138,#7494,#7495);
#5970=AXIS2_PLACEMENT_3D('',#9140,#7497,#7498);
#5971=AXIS2_PLACEMENT_3D('',#9142,#7500,#7501);
#5972=AXIS2_PLACEMENT_3D('',#9143,#7502,#7503);
#5973=AXIS2_PLACEMENT_3D('',#9145,#7505,#7506);
#5974=AXIS2_PLACEMENT_3D('',#9147,#7508,#7509);
#5975=AXIS2_PLACEMENT_3D('',#9149,#7511,#7512);
#5976=AXIS2_PLACEMENT_3D('',#9151,#7514,#7515);
#5977=AXIS2_PLACEMENT_3D('',#9152,#7516,#7517);
#5978=AXIS2_PLACEMENT_3D('',#9154,#7519,#7520);
#5979=AXIS2_PLACEMENT_3D('',#9156,#7522,#7523);
#5980=AXIS2_PLACEMENT_3D('',#9158,#7525,#7526);
#5981=AXIS2_PLACEMENT_3D('',#9160,#7528,#7529);
#5982=AXIS2_PLACEMENT_3D('',#9161,#7530,#7531);
#5983=AXIS2_PLACEMENT_3D('',#9163,#7533,#7534);
#5984=AXIS2_PLACEMENT_3D('',#9165,#7536,#7537);
#5985=AXIS2_PLACEMENT_3D('',#9167,#7539,#7540);
#5986=AXIS2_PLACEMENT_3D('',#9169,#7542,#7543);
#5987=AXIS2_PLACEMENT_3D('',#9170,#7544,#7545);
#5988=AXIS2_PLACEMENT_3D('',#9172,#7547,#7548);
#5989=AXIS2_PLACEMENT_3D('',#9174,#7550,#7551);
#5990=AXIS2_PLACEMENT_3D('',#9176,#7553,#7554);
#5991=AXIS2_PLACEMENT_3D('',#9178,#7556,#7557);
#5992=AXIS2_PLACEMENT_3D('',#9179,#7558,#7559);
#5993=AXIS2_PLACEMENT_3D('',#9181,#7561,#7562);
#5994=AXIS2_PLACEMENT_3D('',#9183,#7564,#7565);
#5995=AXIS2_PLACEMENT_3D('',#9185,#7567,#7568);
#5996=AXIS2_PLACEMENT_3D('',#9187,#7570,#7571);
#5997=AXIS2_PLACEMENT_3D('',#9188,#7572,#7573);
#5998=AXIS2_PLACEMENT_3D('',#9190,#7575,#7576);
#5999=AXIS2_PLACEMENT_3D('',#9192,#7578,#7579);
#6000=AXIS2_PLACEMENT_3D('',#9194,#7581,#7582);
#6001=AXIS2_PLACEMENT_3D('',#9196,#7584,#7585);
#6002=AXIS2_PLACEMENT_3D('',#9197,#7586,#7587);
#6003=AXIS2_PLACEMENT_3D('',#9199,#7589,#7590);
#6004=AXIS2_PLACEMENT_3D('',#9201,#7592,#7593);
#6005=AXIS2_PLACEMENT_3D('',#9203,#7595,#7596);
#6006=AXIS2_PLACEMENT_3D('',#9205,#7598,#7599);
#6007=AXIS2_PLACEMENT_3D('',#9206,#7600,#7601);
#6008=AXIS2_PLACEMENT_3D('',#9208,#7603,#7604);
#6009=AXIS2_PLACEMENT_3D('',#9210,#7606,#7607);
#6010=AXIS2_PLACEMENT_3D('',#9212,#7609,#7610);
#6011=AXIS2_PLACEMENT_3D('',#9214,#7612,#7613);
#6012=AXIS2_PLACEMENT_3D('',#9215,#7614,#7615);
#6013=AXIS2_PLACEMENT_3D('',#9218,#7618,#7619);
#6014=AXIS2_PLACEMENT_3D('',#9219,#7620,#7621);
#6015=AXIS2_PLACEMENT_3D('',#9220,#7622,#7623);
#6016=AXIS2_PLACEMENT_3D('',#9221,#7624,#7625);
#6017=AXIS2_PLACEMENT_3D('',#9223,#7626,#7627);
#6018=AXIS2_PLACEMENT_3D('',#9226,#7629,#7630);
#6019=AXIS2_PLACEMENT_3D('',#9227,#7631,#7632);
#6020=AXIS2_PLACEMENT_3D('',#9230,#7633,#7634);
#6021=AXIS2_PLACEMENT_3D('',#9238,#7635,#7636);
#6022=AXIS2_PLACEMENT_3D('',#9241,#7637,#7638);
#6023=AXIS2_PLACEMENT_3D('',#9249,#7639,#7640);
#6024=AXIS2_PLACEMENT_3D('',#9260,#7643,#7644);
#6025=AXIS2_PLACEMENT_3D('',#9270,#7646,#7647);
#6026=AXIS2_PLACEMENT_3D('',#9288,#7649,#7650);
#6027=AXIS2_PLACEMENT_3D('',#9306,#7652,#7653);
#6028=AXIS2_PLACEMENT_3D('',#9324,#7655,#7656);
#6029=AXIS2_PLACEMENT_3D('',#9339,#7657,#7658);
#6030=AXIS2_PLACEMENT_3D('',#9340,#7659,#7660);
#6031=AXIS2_PLACEMENT_3D('',#9341,#7661,#7662);
#6032=AXIS2_PLACEMENT_3D('',#9342,#7663,#7664);
#6033=AXIS2_PLACEMENT_3D('',#9343,#7665,#7666);
#6034=AXIS2_PLACEMENT_3D('',#9344,#7667,#7668);
#6035=AXIS2_PLACEMENT_3D('',#9345,#7669,#7670);
#6036=AXIS2_PLACEMENT_3D('',#9346,#7671,#7672);
#6037=AXIS2_PLACEMENT_3D('',#9347,#7673,#7674);
#6038=AXIS2_PLACEMENT_3D('',#9348,#7675,#7676);
#6039=AXIS2_PLACEMENT_3D('',#9349,#7677,#7678);
#6040=AXIS2_PLACEMENT_3D('',#9350,#7679,#7680);
#6041=AXIS2_PLACEMENT_3D('',#9351,#7681,#7682);
#6042=AXIS2_PLACEMENT_3D('',#9352,#7683,#7684);
#6043=AXIS2_PLACEMENT_3D('',#9353,#7685,#7686);
#6044=AXIS2_PLACEMENT_3D('',#9354,#7687,#7688);
#6045=AXIS2_PLACEMENT_3D('',#9355,#7689,#7690);
#6046=AXIS2_PLACEMENT_3D('',#9356,#7691,#7692);
#6047=AXIS2_PLACEMENT_3D('',#9357,#7693,#7694);
#6048=AXIS2_PLACEMENT_3D('',#9358,#7695,#7696);
#6049=AXIS2_PLACEMENT_3D('',#9359,#7697,#7698);
#6050=AXIS2_PLACEMENT_3D('',#9360,#7699,#7700);
#6051=AXIS2_PLACEMENT_3D('',#9361,#7701,#7702);
#6052=AXIS2_PLACEMENT_3D('',#9362,#7703,#7704);
#6053=AXIS2_PLACEMENT_3D('',#9364,#7705,#7706);
#6054=AXIS2_PLACEMENT_3D('',#9367,#7708,#7709);
#6055=AXIS2_PLACEMENT_3D('',#9368,#7710,#7711);
#6056=AXIS2_PLACEMENT_3D('',#9370,#7712,#7713);
#6057=AXIS2_PLACEMENT_3D('',#9373,#7715,#7716);
#6058=AXIS2_PLACEMENT_3D('',#9374,#7717,#7718);
#6059=AXIS2_PLACEMENT_3D('',#9376,#7719,#7720);
#6060=AXIS2_PLACEMENT_3D('',#9379,#7722,#7723);
#6061=AXIS2_PLACEMENT_3D('',#9380,#7724,#7725);
#6062=AXIS2_PLACEMENT_3D('',#9382,#7726,#7727);
#6063=AXIS2_PLACEMENT_3D('',#9385,#7729,#7730);
#6064=AXIS2_PLACEMENT_3D('',#9386,#7731,#7732);
#6065=AXIS2_PLACEMENT_3D('',#9388,#7733,#7734);
#6066=AXIS2_PLACEMENT_3D('',#9391,#7736,#7737);
#6067=AXIS2_PLACEMENT_3D('',#9392,#7738,#7739);
#6068=AXIS2_PLACEMENT_3D('',#9394,#7740,#7741);
#6069=AXIS2_PLACEMENT_3D('',#9397,#7743,#7744);
#6070=AXIS2_PLACEMENT_3D('',#9398,#7745,#7746);
#6071=AXIS2_PLACEMENT_3D('',#9400,#7747,#7748);
#6072=AXIS2_PLACEMENT_3D('',#9403,#7750,#7751);
#6073=AXIS2_PLACEMENT_3D('',#9404,#7752,#7753);
#6074=AXIS2_PLACEMENT_3D('',#9405,#7754,#7755);
#6075=AXIS2_PLACEMENT_3D('',#9406,#7756,#7757);
#6076=AXIS2_PLACEMENT_3D('',#9407,#7758,#7759);
#6077=AXIS2_PLACEMENT_3D('',#9408,#7760,#7761);
#6078=AXIS2_PLACEMENT_3D('',#9410,#7762,#7763);
#6079=AXIS2_PLACEMENT_3D('',#9413,#7765,#7766);
#6080=AXIS2_PLACEMENT_3D('',#9414,#7767,#7768);
#6081=AXIS2_PLACEMENT_3D('',#9416,#7769,#7770);
#6082=AXIS2_PLACEMENT_3D('',#9419,#7772,#7773);
#6083=AXIS2_PLACEMENT_3D('',#9420,#7774,#7775);
#6084=AXIS2_PLACEMENT_3D('',#9421,#7776,#7777);
#6085=AXIS2_PLACEMENT_3D('',#9422,#7778,#7779);
#6086=AXIS2_PLACEMENT_3D('',#9423,#7780,#7781);
#6087=AXIS2_PLACEMENT_3D('',#9425,#7782,#7783);
#6088=AXIS2_PLACEMENT_3D('',#9428,#7785,#7786);
#6089=AXIS2_PLACEMENT_3D('',#9429,#7787,#7788);
#6090=AXIS2_PLACEMENT_3D('',#9442,#7795,#7796);
#6091=AXIS2_PLACEMENT_3D('',#9448,#7800,#7801);
#6092=AXIS2_PLACEMENT_3D('',#9452,#7804,#7805);
#6093=AXIS2_PLACEMENT_3D('',#9456,#7808,#7809);
#6094=AXIS2_PLACEMENT_3D('',#9460,#7812,#7813);
#6095=AXIS2_PLACEMENT_3D('',#9464,#7816,#7817);
#6096=AXIS2_PLACEMENT_3D('',#9466,#7819,#7820);
#6097=AXIS2_PLACEMENT_3D('',#9467,#7821,#7822);
#6098=AXIS2_PLACEMENT_3D('',#9468,#7823,#7824);
#6099=AXIS2_PLACEMENT_3D('',#9469,#7825,#7826);
#6100=AXIS2_PLACEMENT_3D('',#9486,#7828,#7829);
#6101=AXIS2_PLACEMENT_3D('',#9500,#7830,#7831);
#6102=AXIS2_PLACEMENT_3D('',#9538,#7833,#7834);
#6103=AXIS2_PLACEMENT_3D('',#9576,#7836,#7837);
#6104=AXIS2_PLACEMENT_3D('',#9589,#7839,#7840);
#6105=AXIS2_PLACEMENT_3D('',#9599,#7841,#7842);
#6106=AXIS2_PLACEMENT_3D('',#9604,#7844,#7845);
#6107=AXIS2_PLACEMENT_3D('',#9618,#7846,#7847);
#6108=AXIS2_PLACEMENT_3D('',#9619,#7848,#7849);
#6109=AXIS2_PLACEMENT_3D('',#9639,#7851,#7852);
#6110=AXIS2_PLACEMENT_3D('',#9651,#7853,#7854);
#6111=AXIS2_PLACEMENT_3D('',#9652,#7855,#7856);
#6112=AXIS2_PLACEMENT_3D('',#9720,#7858,#7859);
#6113=AXIS2_PLACEMENT_3D('',#9796,#7861,#7862);
#6114=AXIS2_PLACEMENT_3D('',#9818,#7864,#7865);
#6115=AXIS2_PLACEMENT_3D('',#9891,#7866,#7867);
#6116=AXIS2_PLACEMENT_3D('',#9911,#7869,#7870);
#6117=AXIS2_PLACEMENT_3D('',#9923,#7871,#7872);
#6118=AXIS2_PLACEMENT_3D('',#9925,#7873,#7874);
#6119=AXIS2_PLACEMENT_3D('',#9952,#7875,#7876);
#6120=AXIS2_PLACEMENT_3D('',#9954,#7877,#7878);
#6121=AXIS2_PLACEMENT_3D('',#9989,#7879,#7880);
#6122=AXIS2_PLACEMENT_3D('',#10002,#7887,#7888);
#6123=AXIS2_PLACEMENT_3D('',#10003,#7889,#7890);
#6124=AXIS2_PLACEMENT_3D('',#10004,#7891,#7892);
#6125=AXIS2_PLACEMENT_3D('',#10005,#7893,#7894);
#6126=AXIS2_PLACEMENT_3D('',#10006,#7895,#7896);
#6127=AXIS2_PLACEMENT_3D('',#10007,#7897,#7898);
#6128=AXIS2_PLACEMENT_3D('',#10010,#7901,#7902);
#6129=AXIS2_PLACEMENT_3D('',#10012,#7904,#7905);
#6130=AXIS2_PLACEMENT_3D('',#10014,#7907,#7908);
#6131=AXIS2_PLACEMENT_3D('',#10016,#7910,#7911);
#6132=AXIS2_PLACEMENT_3D('',#10018,#7913,#7914);
#6133=AXIS2_PLACEMENT_3D('',#10019,#7915,#7916);
#6134=AXIS2_PLACEMENT_3D('',#10378,#7917,#7918);
#6135=AXIS2_PLACEMENT_3D('',#10379,#7919,#7920);
#6136=AXIS2_PLACEMENT_3D('',#10380,#7921,#7922);
#6137=AXIS2_PLACEMENT_3D('',#10381,#7923,#7924);
#6138=AXIS2_PLACEMENT_3D('',#10382,#7925,#7926);
#6139=AXIS2_PLACEMENT_3D('',#10383,#7927,#7928);
#6140=AXIS2_PLACEMENT_3D('',#10384,#7929,#7930);
#6141=AXIS2_PLACEMENT_3D('',#10385,#7931,#7932);
#6142=AXIS2_PLACEMENT_3D('',#10386,#7933,#7934);
#6143=AXIS2_PLACEMENT_3D('',#10387,#7935,#7936);
#6144=AXIS2_PLACEMENT_3D('',#10388,#7937,#7938);
#6145=AXIS2_PLACEMENT_3D('',#10389,#7939,#7940);
#6146=AXIS2_PLACEMENT_3D('',#10390,#7941,#7942);
#6147=AXIS2_PLACEMENT_3D('',#10391,#7943,#7944);
#6148=AXIS2_PLACEMENT_3D('',#10392,#7945,#7946);
#6149=AXIS2_PLACEMENT_3D('',#10393,#7947,#7948);
#6150=DIRECTION('axis',(0.,0.,1.));
#6151=DIRECTION('refdir',(1.,0.,0.));
#6152=DIRECTION('axis',(0.,0.,1.));
#6153=DIRECTION('refdir',(1.,0.,0.));
#6154=DIRECTION('center_axis',(-1.,0.,0.));
#6155=DIRECTION('ref_axis',(0.,0.,1.));
#6156=DIRECTION('center_axis',(-1.,0.,0.));
#6157=DIRECTION('ref_axis',(0.,0.,1.));
#6158=DIRECTION('',(-1.,0.,0.));
#6159=DIRECTION('center_axis',(-1.,0.,0.));
#6160=DIRECTION('ref_axis',(0.,0.,1.));
#6161=DIRECTION('center_axis',(-1.,0.,0.));
#6162=DIRECTION('ref_axis',(0.,0.,1.));
#6163=DIRECTION('center_axis',(-1.,0.,0.));
#6164=DIRECTION('ref_axis',(0.,0.,1.));
#6165=DIRECTION('',(-1.,0.,0.));
#6166=DIRECTION('center_axis',(-1.,0.,0.));
#6167=DIRECTION('ref_axis',(0.,0.,1.));
#6168=DIRECTION('center_axis',(0.,0.,1.));
#6169=DIRECTION('ref_axis',(1.,0.,0.));
#6170=DIRECTION('center_axis',(0.,0.,-1.));
#6171=DIRECTION('ref_axis',(-1.,0.,0.));
#6172=DIRECTION('',(0.,0.,1.));
#6173=DIRECTION('center_axis',(0.,0.,1.));
#6174=DIRECTION('ref_axis',(1.,0.,0.));
#6175=DIRECTION('center_axis',(0.,0.,-1.));
#6176=DIRECTION('ref_axis',(-1.,0.,0.));
#6177=DIRECTION('center_axis',(0.,0.,1.));
#6178=DIRECTION('ref_axis',(1.,0.,0.));
#6179=DIRECTION('',(0.,0.,-1.));
#6180=DIRECTION('center_axis',(0.,0.,1.));
#6181=DIRECTION('ref_axis',(1.,0.,0.));
#6182=DIRECTION('center_axis',(0.,0.,1.));
#6183=DIRECTION('ref_axis',(1.,0.,0.));
#6184=DIRECTION('center_axis',(0.,0.,1.));
#6185=DIRECTION('ref_axis',(1.,0.,0.));
#6186=DIRECTION('',(0.,0.,1.));
#6187=DIRECTION('center_axis',(0.,0.,1.));
#6188=DIRECTION('ref_axis',(1.,0.,0.));
#6189=DIRECTION('center_axis',(0.,0.,1.));
#6190=DIRECTION('ref_axis',(1.,0.,0.));
#6191=DIRECTION('center_axis',(0.,0.,1.));
#6192=DIRECTION('ref_axis',(1.,0.,0.));
#6193=DIRECTION('',(0.,0.,1.));
#6194=DIRECTION('center_axis',(0.,0.,1.));
#6195=DIRECTION('ref_axis',(1.,0.,0.));
#6196=DIRECTION('center_axis',(0.,0.,1.));
#6197=DIRECTION('ref_axis',(1.,0.,0.));
#6198=DIRECTION('center_axis',(0.,0.,1.));
#6199=DIRECTION('ref_axis',(1.,0.,0.));
#6200=DIRECTION('',(0.,0.,1.));
#6201=DIRECTION('center_axis',(0.,0.,1.));
#6202=DIRECTION('ref_axis',(1.,0.,0.));
#6203=DIRECTION('center_axis',(0.,0.,1.));
#6204=DIRECTION('ref_axis',(1.,0.,0.));
#6205=DIRECTION('center_axis',(0.,0.,1.));
#6206=DIRECTION('ref_axis',(1.,0.,0.));
#6207=DIRECTION('',(0.,0.,1.));
#6208=DIRECTION('center_axis',(0.,0.,1.));
#6209=DIRECTION('ref_axis',(1.,0.,0.));
#6210=DIRECTION('center_axis',(0.,0.,1.));
#6211=DIRECTION('ref_axis',(1.,0.,0.));
#6212=DIRECTION('center_axis',(0.,0.,1.));
#6213=DIRECTION('ref_axis',(1.,0.,0.));
#6214=DIRECTION('',(0.,0.,1.));
#6215=DIRECTION('center_axis',(0.,0.,1.));
#6216=DIRECTION('ref_axis',(1.,0.,0.));
#6217=DIRECTION('center_axis',(0.,0.,-1.));
#6218=DIRECTION('ref_axis',(-1.,0.,0.));
#6219=DIRECTION('',(0.,-1.,0.));
#6220=DIRECTION('',(-1.,0.,0.));
#6221=DIRECTION('',(1.73472347597681E-17,1.,0.));
#6222=DIRECTION('',(1.,0.,0.));
#6223=DIRECTION('center_axis',(0.,0.,-1.));
#6224=DIRECTION('ref_axis',(-1.,0.,0.));
#6225=DIRECTION('',(-1.73472347597681E-17,-1.,0.));
#6226=DIRECTION('',(-1.,0.,0.));
#6227=DIRECTION('',(0.,1.,0.));
#6228=DIRECTION('',(1.,0.,0.));
#6229=DIRECTION('center_axis',(0.,1.,0.));
#6230=DIRECTION('ref_axis',(0.,0.,1.));
#6231=DIRECTION('',(0.,0.,1.));
#6232=DIRECTION('',(0.,0.,1.));
#6233=DIRECTION('',(1.,1.22464679914735E-16,0.));
#6234=DIRECTION('',(0.,0.,-1.));
#6235=DIRECTION('center_axis',(0.,-1.,0.));
#6236=DIRECTION('ref_axis',(0.,0.,-1.));
#6237=DIRECTION('',(0.,0.,1.));
#6238=DIRECTION('',(0.,0.,-1.));
#6239=DIRECTION('',(-1.,0.,0.));
#6240=DIRECTION('',(0.,0.,1.));
#6241=DIRECTION('center_axis',(0.,0.,1.));
#6242=DIRECTION('ref_axis',(1.,0.,0.));
#6243=DIRECTION('center_axis',(0.,0.,-1.));
#6244=DIRECTION('ref_axis',(1.,0.,0.));
#6245=DIRECTION('center_axis',(1.,-1.73472347597681E-17,0.));
#6246=DIRECTION('ref_axis',(1.73472347597681E-17,1.,0.));
#6247=DIRECTION('center_axis',(1.,0.,0.));
#6248=DIRECTION('ref_axis',(0.,0.,-1.));
#6249=DIRECTION('',(0.,1.,0.));
#6250=DIRECTION('center_axis',(1.,0.,0.));
#6251=DIRECTION('ref_axis',(0.,0.,-1.));
#6252=DIRECTION('',(0.,-1.,0.));
#6253=DIRECTION('center_axis',(0.,0.,-1.));
#6254=DIRECTION('ref_axis',(-1.,0.,0.));
#6255=DIRECTION('axis',(0.,0.,1.));
#6256=DIRECTION('refdir',(1.,0.,0.));
#6257=DIRECTION('center_axis',(0.,0.,-1.));
#6258=DIRECTION('ref_axis',(-1.,0.,0.));
#6259=DIRECTION('center_axis',(0.,0.,1.));
#6260=DIRECTION('ref_axis',(1.,0.,0.));
#6261=DIRECTION('',(0.,0.,1.));
#6262=DIRECTION('center_axis',(0.,0.,1.));
#6263=DIRECTION('ref_axis',(1.,0.,0.));
#6264=DIRECTION('center_axis',(0.,0.,-1.));
#6265=DIRECTION('ref_axis',(-1.,0.,0.));
#6266=DIRECTION('center_axis',(0.,0.,1.));
#6267=DIRECTION('ref_axis',(1.,0.,0.));
#6268=DIRECTION('',(0.,0.,-1.));
#6269=DIRECTION('center_axis',(0.,0.,1.));
#6270=DIRECTION('ref_axis',(1.,0.,0.));
#6271=DIRECTION('',(0.,0.,1.));
#6272=DIRECTION('center_axis',(0.,0.,1.));
#6273=DIRECTION('ref_axis',(1.,0.,0.));
#6274=DIRECTION('center_axis',(0.,0.,1.));
#6275=DIRECTION('ref_axis',(1.,0.,0.));
#6276=DIRECTION('',(0.,0.,-1.));
#6277=DIRECTION('center_axis',(0.,0.,-1.));
#6278=DIRECTION('ref_axis',(-1.,0.,0.));
#6279=DIRECTION('center_axis',(0.,0.,1.));
#6280=DIRECTION('ref_axis',(1.,0.,0.));
#6281=DIRECTION('',(0.,0.,1.));
#6282=DIRECTION('center_axis',(0.,0.,1.));
#6283=DIRECTION('ref_axis',(1.,0.,0.));
#6284=DIRECTION('center_axis',(0.,0.,1.));
#6285=DIRECTION('ref_axis',(1.,0.,0.));
#6286=DIRECTION('center_axis',(0.,0.,1.));
#6287=DIRECTION('ref_axis',(1.,0.,0.));
#6288=DIRECTION('center_axis',(0.,0.,-1.));
#6289=DIRECTION('ref_axis',(-1.,0.,0.));
#6290=DIRECTION('center_axis',(0.,0.,1.));
#6291=DIRECTION('ref_axis',(1.,0.,0.));
#6292=DIRECTION('',(0.,0.,1.));
#6293=DIRECTION('center_axis',(0.,0.,1.));
#6294=DIRECTION('ref_axis',(1.,0.,0.));
#6295=DIRECTION('center_axis',(0.,0.,-1.));
#6296=DIRECTION('ref_axis',(-1.,0.,0.));
#6297=DIRECTION('center_axis',(0.,0.,1.));
#6298=DIRECTION('ref_axis',(1.,0.,0.));
#6299=DIRECTION('',(0.,0.,1.));
#6300=DIRECTION('center_axis',(0.,0.,1.));
#6301=DIRECTION('ref_axis',(1.,0.,0.));
#6302=DIRECTION('center_axis',(0.,0.,1.));
#6303=DIRECTION('ref_axis',(1.,0.,0.));
#6304=DIRECTION('center_axis',(0.,0.,1.));
#6305=DIRECTION('ref_axis',(1.,0.,0.));
#6306=DIRECTION('center_axis',(0.,0.,1.));
#6307=DIRECTION('ref_axis',(1.,0.,0.));
#6308=DIRECTION('center_axis',(0.,0.,1.));
#6309=DIRECTION('ref_axis',(1.,0.,0.));
#6310=DIRECTION('center_axis',(0.,0.,1.));
#6311=DIRECTION('ref_axis',(1.,0.,0.));
#6312=DIRECTION('',(-1.,0.,0.));
#6313=DIRECTION('',(1.,0.,0.));
#6314=DIRECTION('center_axis',(0.,0.,1.));
#6315=DIRECTION('ref_axis',(1.,0.,0.));
#6316=DIRECTION('',(-1.,0.,0.));
#6317=DIRECTION('',(1.,0.,0.));
#6318=DIRECTION('',(0.,-1.,0.));
#6319=DIRECTION('center_axis',(0.,-1.,0.));
#6320=DIRECTION('ref_axis',(0.,0.,-1.));
#6321=DIRECTION('',(0.,0.,-1.));
#6322=DIRECTION('',(-1.,0.,0.));
#6323=DIRECTION('center_axis',(1.,0.,0.));
#6324=DIRECTION('ref_axis',(0.,0.,-1.));
#6325=DIRECTION('',(0.,0.,-1.));
#6326=DIRECTION('',(0.,-1.,0.));
#6327=DIRECTION('center_axis',(0.,1.,0.));
#6328=DIRECTION('ref_axis',(0.,0.,1.));
#6329=DIRECTION('',(1.,0.,0.));
#6330=DIRECTION('center_axis',(0.,0.,1.));
#6331=DIRECTION('ref_axis',(1.,0.,0.));
#6332=DIRECTION('center_axis',(0.,0.,1.));
#6333=DIRECTION('ref_axis',(1.,0.,0.));
#6334=DIRECTION('axis',(0.,0.,1.));
#6335=DIRECTION('refdir',(1.,0.,0.));
#6336=DIRECTION('center_axis',(0.,0.,1.));
#6337=DIRECTION('ref_axis',(7.80990875742903E-15,-1.,0.));
#6338=DIRECTION('center_axis',(0.,0.,1.));
#6339=DIRECTION('ref_axis',(1.,0.,0.));
#6340=DIRECTION('',(0.,0.,1.));
#6341=DIRECTION('center_axis',(0.,0.,1.));
#6342=DIRECTION('ref_axis',(1.,0.,0.));
#6343=DIRECTION('',(0.,0.,-1.));
#6344=DIRECTION('center_axis',(0.,0.,-1.));
#6345=DIRECTION('ref_axis',(-1.,0.,0.));
#6346=DIRECTION('center_axis',(0.,0.,-1.));
#6347=DIRECTION('ref_axis',(-1.,0.,0.));
#6348=DIRECTION('',(0.,0.,1.));
#6349=DIRECTION('center_axis',(0.,0.,1.));
#6350=DIRECTION('ref_axis',(1.,0.,0.));
#6351=DIRECTION('',(0.,0.,-1.));
#6352=DIRECTION('center_axis',(0.,0.,1.));
#6353=DIRECTION('ref_axis',(1.,0.,0.));
#6354=DIRECTION('center_axis',(1.78945947642876E-15,2.74818654191516E-16,
-1.));
#6355=DIRECTION('ref_axis',(-1.,-3.8094332417834E-33,-1.78945947642876E-15));
#6356=DIRECTION('',(0.,0.,-1.));
#6357=DIRECTION('center_axis',(-8.94729738214379E-16,-1.37409327095758E-16,
-1.));
#6358=DIRECTION('ref_axis',(-1.,-9.5235831044585E-34,8.94729738214379E-16));
#6359=DIRECTION('center_axis',(0.,0.,-1.));
#6360=DIRECTION('ref_axis',(-1.,0.,0.));
#6361=DIRECTION('center_axis',(-1.32139904668388E-15,-6.05000891271787E-16,
-1.));
#6362=DIRECTION('ref_axis',(-1.,1.51602385490383E-31,1.32139904668388E-15));
#6363=DIRECTION('',(0.,0.,1.));
#6364=DIRECTION('center_axis',(0.,0.,1.));
#6365=DIRECTION('ref_axis',(1.,0.,0.));
#6366=DIRECTION('',(0.,0.,-1.));
#6367=DIRECTION('center_axis',(0.,0.,1.));
#6368=DIRECTION('ref_axis',(1.,0.,0.));
#6369=DIRECTION('center_axis',(9.03746752270192E-16,-5.16181690799186E-17,
-1.));
#6370=DIRECTION('ref_axis',(-1.,-1.07685893901274E-34,-9.03746752270192E-16));
#6371=DIRECTION('',(0.,0.,-1.));
#6372=DIRECTION('center_axis',(-9.03746752270196E-16,5.16181690799174E-17,
-1.));
#6373=DIRECTION('ref_axis',(-1.,-1.07685893901823E-34,9.03746752270196E-16));
#6374=DIRECTION('center_axis',(0.,0.,-1.));
#6375=DIRECTION('ref_axis',(-1.,0.,0.));
#6376=DIRECTION('center_axis',(0.,0.,-1.));
#6377=DIRECTION('ref_axis',(-1.,0.,0.));
#6378=DIRECTION('',(0.,0.,1.));
#6379=DIRECTION('center_axis',(0.,0.,1.));
#6380=DIRECTION('ref_axis',(1.,0.,0.));
#6381=DIRECTION('',(0.,0.,-1.));
#6382=DIRECTION('center_axis',(0.,0.,1.));
#6383=DIRECTION('ref_axis',(1.,0.,0.));
#6384=DIRECTION('center_axis',(8.94729738214375E-16,-1.37409327095777E-16,
-1.));
#6385=DIRECTION('ref_axis',(-1.,9.52358310447069E-34,-8.94729738214375E-16));
#6386=DIRECTION('center_axis',(-8.94729738214377E-16,1.37409327095776E-16,
-1.));
#6387=DIRECTION('ref_axis',(-1.,9.52358310446614E-34,8.94729738214377E-16));
#6388=DIRECTION('',(0.,0.,1.));
#6389=DIRECTION('center_axis',(0.,0.,-1.));
#6390=DIRECTION('ref_axis',(-1.,0.,0.));
#6391=DIRECTION('center_axis',(0.,0.,-1.));
#6392=DIRECTION('ref_axis',(-1.,0.,0.));
#6393=DIRECTION('',(0.,0.,1.));
#6394=DIRECTION('center_axis',(0.,0.,1.));
#6395=DIRECTION('ref_axis',(1.,0.,0.));
#6396=DIRECTION('',(0.,0.,-1.));
#6397=DIRECTION('center_axis',(0.,0.,1.));
#6398=DIRECTION('ref_axis',(1.,0.,0.));
#6399=DIRECTION('center_axis',(1.80749350454039E-15,1.03236338159802E-16,
-1.));
#6400=DIRECTION('ref_axis',(-1.,4.30743575605734E-34,-1.80749350454039E-15));
#6401=DIRECTION('center_axis',(-1.80749350454039E-15,-1.03236338159807E-16,
-1.));
#6402=DIRECTION('ref_axis',(-1.,4.30743575606245E-34,1.80749350454039E-15));
#6403=DIRECTION('',(0.,0.,1.));
#6404=DIRECTION('center_axis',(0.,0.,-1.));
#6405=DIRECTION('ref_axis',(-1.,0.,0.));
#6406=DIRECTION('center_axis',(0.,0.,-1.));
#6407=DIRECTION('ref_axis',(-1.,0.,0.));
#6408=DIRECTION('',(0.,0.,1.));
#6409=DIRECTION('center_axis',(0.,0.,1.));
#6410=DIRECTION('ref_axis',(1.,0.,0.));
#6411=DIRECTION('',(0.,0.,-1.));
#6412=DIRECTION('center_axis',(0.,0.,-1.));
#6413=DIRECTION('ref_axis',(-1.,0.,0.));
#6414=DIRECTION('center_axis',(0.,0.,-1.));
#6415=DIRECTION('ref_axis',(-1.,0.,0.));
#6416=DIRECTION('',(0.,0.,1.));
#6417=DIRECTION('center_axis',(0.,0.,1.));
#6418=DIRECTION('ref_axis',(1.,0.,0.));
#6419=DIRECTION('',(0.,0.,-1.));
#6420=DIRECTION('center_axis',(0.,0.,-1.));
#6421=DIRECTION('ref_axis',(-1.,0.,0.));
#6422=DIRECTION('center_axis',(0.,0.,-1.));
#6423=DIRECTION('ref_axis',(-1.,0.,0.));
#6424=DIRECTION('',(0.,0.,1.));
#6425=DIRECTION('center_axis',(0.,0.,1.));
#6426=DIRECTION('ref_axis',(1.,0.,0.));
#6427=DIRECTION('',(0.,0.,-1.));
#6428=DIRECTION('center_axis',(0.,0.,-1.));
#6429=DIRECTION('ref_axis',(-1.,0.,0.));
#6430=DIRECTION('center_axis',(0.,0.,-1.));
#6431=DIRECTION('ref_axis',(-1.,0.,0.));
#6432=DIRECTION('',(0.,0.,1.));
#6433=DIRECTION('center_axis',(0.,0.,1.));
#6434=DIRECTION('ref_axis',(1.,0.,0.));
#6435=DIRECTION('',(0.,0.,-1.));
#6436=DIRECTION('center_axis',(0.,0.,-1.));
#6437=DIRECTION('ref_axis',(-1.,0.,0.));
#6438=DIRECTION('center_axis',(1.18464566449559E-15,8.4186469732886E-16,
-1.));
#6439=DIRECTION('ref_axis',(-1.,9.5828367453829E-32,-1.18464566449559E-15));
#6440=DIRECTION('',(0.,0.,1.));
#6441=DIRECTION('center_axis',(1.18464566449559E-15,8.4186469732886E-16,
1.));
#6442=DIRECTION('ref_axis',(1.,-9.5828367453829E-32,-1.18464566449559E-15));
#6443=DIRECTION('',(0.,0.,-1.));
#6444=DIRECTION('center_axis',(0.,0.,-1.));
#6445=DIRECTION('ref_axis',(-1.,0.,0.));
#6446=DIRECTION('center_axis',(0.,0.,-1.));
#6447=DIRECTION('ref_axis',(-1.,0.,0.));
#6448=DIRECTION('',(0.,0.,1.));
#6449=DIRECTION('center_axis',(0.,0.,1.));
#6450=DIRECTION('ref_axis',(1.,0.,0.));
#6451=DIRECTION('',(0.,0.,-1.));
#6452=DIRECTION('center_axis',(0.,0.,-1.));
#6453=DIRECTION('ref_axis',(-1.,0.,0.));
#6454=DIRECTION('center_axis',(-1.45323412840511E-15,-1.52344036793038E-17,
-1.));
#6455=DIRECTION('ref_axis',(-1.,-2.33073141121972E-33,1.45323412840511E-15));
#6456=DIRECTION('',(0.,0.,1.));
#6457=DIRECTION('center_axis',(0.,0.,1.));
#6458=DIRECTION('ref_axis',(1.,0.,0.));
#6459=DIRECTION('',(0.,0.,-1.));
#6460=DIRECTION('center_axis',(0.,0.,-1.));
#6461=DIRECTION('ref_axis',(-1.,0.,0.));
#6462=DIRECTION('center_axis',(0.,0.,-1.));
#6463=DIRECTION('ref_axis',(-1.,0.,0.));
#6464=DIRECTION('',(0.,0.,1.));
#6465=DIRECTION('center_axis',(0.,0.,1.));
#6466=DIRECTION('ref_axis',(1.,0.,0.));
#6467=DIRECTION('',(0.,0.,-1.));
#6468=DIRECTION('center_axis',(0.,0.,-1.));
#6469=DIRECTION('ref_axis',(-1.,0.,0.));
#6470=DIRECTION('center_axis',(-1.42464488663145E-15,2.87242869383234E-16,
-1.));
#6471=DIRECTION('ref_axis',(-1.,5.21577193803856E-32,1.42464488663145E-15));
#6472=DIRECTION('',(0.,0.,1.));
#6473=DIRECTION('center_axis',(-1.42464488663145E-15,2.87242869383234E-16,
1.));
#6474=DIRECTION('ref_axis',(1.,-5.21577193803856E-32,1.42464488663145E-15));
#6475=DIRECTION('',(0.,0.,-1.));
#6476=DIRECTION('center_axis',(0.,0.,-1.));
#6477=DIRECTION('ref_axis',(-1.,0.,0.));
#6478=DIRECTION('center_axis',(0.,0.,-1.));
#6479=DIRECTION('ref_axis',(-1.,0.,0.));
#6480=DIRECTION('',(0.,0.,1.));
#6481=DIRECTION('center_axis',(0.,0.,1.));
#6482=DIRECTION('ref_axis',(1.,0.,0.));
#6483=DIRECTION('',(0.,0.,-1.));
#6484=DIRECTION('center_axis',(0.,0.,-1.));
#6485=DIRECTION('ref_axis',(-1.,0.,0.));
#6486=DIRECTION('center_axis',(-5.29913193257237E-14,0.,1.));
#6487=DIRECTION('ref_axis',(1.,0.,5.29913193257237E-14));
#6488=DIRECTION('',(0.,0.,-1.));
#6489=DIRECTION('center_axis',(5.29913193257013E-14,0.,1.));
#6490=DIRECTION('ref_axis',(1.,0.,-5.29913193257013E-14));
#6491=DIRECTION('',(0.,0.,1.));
#6492=DIRECTION('center_axis',(0.,0.,-1.));
#6493=DIRECTION('ref_axis',(-1.,0.,0.));
#6494=DIRECTION('center_axis',(-3.54581136321782E-14,-3.93802247521328E-14,
1.));
#6495=DIRECTION('ref_axis',(-8.56410064059132E-32,-1.,-3.93802247521328E-14));
#6496=DIRECTION('',(0.,0.,-1.));
#6497=DIRECTION('center_axis',(3.54581136321784E-14,3.93802247521327E-14,
1.));
#6498=DIRECTION('ref_axis',(-8.56410063443906E-32,-1.,3.93802247521327E-14));
#6499=DIRECTION('',(0.,0.,1.));
#6500=DIRECTION('center_axis',(0.,0.,-1.));
#6501=DIRECTION('ref_axis',(-1.,0.,0.));
#6502=DIRECTION('center_axis',(4.28708778888507E-14,3.11475159991745E-14,
1.));
#6503=DIRECTION('ref_axis',(1.,-1.47528330080296E-31,-4.28708778888507E-14));
#6504=DIRECTION('',(0.,0.,1.));
#6505=DIRECTION('center_axis',(-4.28708778888507E-14,-3.11475159991745E-14,
1.));
#6506=DIRECTION('ref_axis',(1.,-1.47528330080296E-31,4.28708778888507E-14));
#6507=DIRECTION('',(0.,0.,-1.));
#6508=DIRECTION('center_axis',(0.,0.,-1.));
#6509=DIRECTION('ref_axis',(-1.,0.,0.));
#6510=DIRECTION('center_axis',(-2.64956596628557E-14,-4.58918287161186E-14,
1.));
#6511=DIRECTION('ref_axis',(1.05337643511338E-31,-1.,-4.58918287161186E-14));
#6512=DIRECTION('',(0.,0.,-1.));
#6513=DIRECTION('center_axis',(2.64956596628557E-14,4.58918287161186E-14,
1.));
#6514=DIRECTION('ref_axis',(1.05337643511338E-31,-1.,4.58918287161186E-14));
#6515=DIRECTION('',(0.,0.,1.));
#6516=DIRECTION('center_axis',(0.,0.,-1.));
#6517=DIRECTION('ref_axis',(-1.,0.,0.));
#6518=DIRECTION('center_axis',(-1.63752182259927E-14,-5.03977395517881E-14,
1.));
#6519=DIRECTION('ref_axis',(3.95682458153076E-32,-1.,-5.03977395517881E-14));
#6520=DIRECTION('',(0.,0.,-1.));
#6521=DIRECTION('center_axis',(1.63752182259958E-14,5.03977395517984E-14,
1.));
#6522=DIRECTION('ref_axis',(3.95682460883029E-32,-1.,5.03977395517984E-14));
#6523=DIRECTION('',(0.,0.,1.));
#6524=DIRECTION('center_axis',(0.,0.,-1.));
#6525=DIRECTION('ref_axis',(-1.,0.,0.));
#6526=DIRECTION('center_axis',(4.84099790645001E-14,2.1553511334701E-14,
1.));
#6527=DIRECTION('ref_axis',(1.,-5.08629423737342E-32,-4.84099790645001E-14));
#6528=DIRECTION('',(0.,0.,1.));
#6529=DIRECTION('center_axis',(-4.84099790645117E-14,-2.1553511334706E-14,
1.));
#6530=DIRECTION('ref_axis',(1.,-5.08629429118651E-32,4.84099790645117E-14));
#6531=DIRECTION('',(0.,0.,-1.));
#6532=DIRECTION('center_axis',(0.,0.,-1.));
#6533=DIRECTION('ref_axis',(-1.,0.,0.));
#6534=DIRECTION('center_axis',(5.18333318581752E-14,1.1017514799675E-14,
1.));
#6535=DIRECTION('ref_axis',(1.,-2.69341656657878E-32,-5.18333318581752E-14));
#6536=DIRECTION('',(0.,0.,1.));
#6537=DIRECTION('center_axis',(-5.18333318581731E-14,-1.10175147996738E-14,
1.));
#6538=DIRECTION('ref_axis',(1.,-2.69341656387513E-32,5.18333318581731E-14));
#6539=DIRECTION('',(0.,0.,-1.));
#6540=DIRECTION('center_axis',(0.,0.,-1.));
#6541=DIRECTION('ref_axis',(-1.,0.,0.));
#6542=DIRECTION('center_axis',(5.18333318581723E-14,-1.10175147996744E-14,
1.));
#6543=DIRECTION('ref_axis',(1.,2.6934165598586E-32,-5.18333318581723E-14));
#6544=DIRECTION('',(0.,0.,1.));
#6545=DIRECTION('center_axis',(-5.18333318581729E-14,1.10175147996745E-14,
1.));
#6546=DIRECTION('ref_axis',(1.,2.69341656220821E-32,5.18333318581729E-14));
#6547=DIRECTION('',(0.,0.,-1.));
#6548=DIRECTION('center_axis',(0.,0.,-1.));
#6549=DIRECTION('ref_axis',(-1.,0.,0.));
#6550=DIRECTION('center_axis',(-2.64956596628442E-14,4.58918287160994E-14,
1.));
#6551=DIRECTION('ref_axis',(-1.053376425146E-31,-1.,4.58918287160994E-14));
#6552=DIRECTION('',(0.,0.,-1.));
#6553=DIRECTION('center_axis',(2.64956596628505E-14,-4.58918287161103E-14,
1.));
#6554=DIRECTION('ref_axis',(-1.05337643066151E-31,-1.,-4.58918287161103E-14));
#6555=DIRECTION('',(0.,0.,1.));
#6556=DIRECTION('center_axis',(0.,0.,-1.));
#6557=DIRECTION('ref_axis',(-1.,0.,0.));
#6558=DIRECTION('center_axis',(-3.54581136321834E-14,3.93802247521383E-14,
1.));
#6559=DIRECTION('ref_axis',(8.56410059928329E-32,-1.,3.93802247521383E-14));
#6560=DIRECTION('',(0.,0.,-1.));
#6561=DIRECTION('center_axis',(3.54581136321726E-14,-3.93802247521266E-14,
1.));
#6562=DIRECTION('ref_axis',(8.56410068268857E-32,-1.,-3.93802247521266E-14));
#6563=DIRECTION('',(0.,0.,1.));
#6564=DIRECTION('center_axis',(0.,0.,-1.));
#6565=DIRECTION('ref_axis',(-1.,0.,0.));
#6566=DIRECTION('center_axis',(4.8409979064475E-14,-2.15535113346903E-14,
1.));
#6567=DIRECTION('ref_axis',(1.,5.08629413077073E-32,-4.8409979064475E-14));
#6568=DIRECTION('',(0.,0.,1.));
#6569=DIRECTION('center_axis',(-4.84099790644917E-14,2.15535113346974E-14,
1.));
#6570=DIRECTION('ref_axis',(1.,5.08629420584556E-32,4.84099790644917E-14));
#6571=DIRECTION('',(0.,0.,-1.));
#6572=DIRECTION('center_axis',(0.,0.,-1.));
#6573=DIRECTION('ref_axis',(-1.,0.,0.));
#6574=DIRECTION('center_axis',(4.28708778888503E-14,-3.11475159991748E-14,
1.));
#6575=DIRECTION('ref_axis',(1.,1.47528330034113E-31,-4.28708778888503E-14));
#6576=DIRECTION('',(0.,0.,1.));
#6577=DIRECTION('center_axis',(-4.28708778888425E-14,3.11475159991688E-14,
1.));
#6578=DIRECTION('ref_axis',(1.,1.47528329562607E-31,4.28708778888425E-14));
#6579=DIRECTION('',(0.,0.,-1.));
#6580=DIRECTION('center_axis',(0.,0.,-1.));
#6581=DIRECTION('ref_axis',(-1.,0.,0.));
#6582=DIRECTION('center_axis',(1.63752182259953E-14,-5.03977395517968E-14,
1.));
#6583=DIRECTION('ref_axis',(-3.95682460334169E-32,-1.,-5.03977395517968E-14));
#6584=DIRECTION('',(0.,0.,1.));
#6585=DIRECTION('center_axis',(-1.63752182259922E-14,5.03977395517884E-14,
1.));
#6586=DIRECTION('ref_axis',(-3.95682457625739E-32,-1.,5.03977395517884E-14));
#6587=DIRECTION('',(0.,0.,-1.));
#6588=DIRECTION('center_axis',(0.,0.,-1.));
#6589=DIRECTION('ref_axis',(-1.,0.,0.));
#6590=DIRECTION('center_axis',(5.53910117564604E-15,-5.27010273339078E-14,
1.));
#6591=DIRECTION('ref_axis',(1.79740491271749E-32,-1.,-5.27010273339078E-14));
#6592=DIRECTION('',(0.,0.,1.));
#6593=DIRECTION('center_axis',(-5.53910117564605E-15,5.27010273339078E-14,
1.));
#6594=DIRECTION('ref_axis',(1.79740491281615E-32,-1.,5.27010273339078E-14));
#6595=DIRECTION('',(0.,0.,-1.));
#6596=DIRECTION('center_axis',(0.,0.,-1.));
#6597=DIRECTION('ref_axis',(-1.,0.,0.));
#6598=DIRECTION('center_axis',(-5.53910117564048E-15,-5.27010273338518E-14,
1.));
#6599=DIRECTION('ref_axis',(-1.79740495843794E-32,-1.,-5.27010273338518E-14));
#6600=DIRECTION('',(0.,0.,1.));
#6601=DIRECTION('center_axis',(5.53910117564134E-15,5.2701027333863E-14,
1.));
#6602=DIRECTION('ref_axis',(-1.79740494549667E-32,-1.,5.2701027333863E-14));
#6603=DIRECTION('center_axis',(0.,0.,-1.));
#6604=DIRECTION('ref_axis',(-1.,0.,0.));
#6605=DIRECTION('center_axis',(-1.63752182259957E-14,-5.03977395517976E-14,
1.));
#6606=DIRECTION('ref_axis',(3.95682460513535E-32,-1.,-5.03977395517976E-14));
#6607=DIRECTION('',(0.,0.,1.));
#6608=DIRECTION('center_axis',(1.63752182259922E-14,5.03977395517865E-14,
1.));
#6609=DIRECTION('ref_axis',(3.956824570141E-32,-1.,5.03977395517865E-14));
#6610=DIRECTION('center_axis',(0.,0.,-1.));
#6611=DIRECTION('ref_axis',(-1.,0.,0.));
#6612=DIRECTION('center_axis',(1.63752182259915E-14,-5.03977395517886E-14,
1.));
#6613=DIRECTION('ref_axis',(-3.95682457867884E-32,-1.,-5.03977395517886E-14));
#6614=DIRECTION('',(0.,0.,-1.));
#6615=DIRECTION('center_axis',(-1.63752182259948E-14,5.03977395517987E-14,
1.));
#6616=DIRECTION('ref_axis',(-3.95682460886617E-32,-1.,5.03977395517987E-14));
#6617=DIRECTION('center_axis',(0.,0.,-1.));
#6618=DIRECTION('ref_axis',(-1.,0.,0.));
#6619=DIRECTION('center_axis',(2.64956596628546E-14,-4.58918287161192E-14,
1.));
#6620=DIRECTION('ref_axis',(-1.053376435221E-31,-1.,-4.58918287161192E-14));
#6621=DIRECTION('',(0.,0.,-1.));
#6622=DIRECTION('center_axis',(-2.64956596628545E-14,4.58918287161191E-14,
1.));
#6623=DIRECTION('ref_axis',(-1.05337643477796E-31,-1.,4.58918287161191E-14));
#6624=DIRECTION('',(0.,0.,1.));
#6625=DIRECTION('center_axis',(0.,0.,-1.));
#6626=DIRECTION('ref_axis',(-1.,0.,0.));
#6627=DIRECTION('center_axis',(4.28708778888447E-14,-3.11475159991715E-14,
1.));
#6628=DIRECTION('ref_axis',(1.,1.47528329704207E-31,-4.28708778888447E-14));
#6629=DIRECTION('',(0.,0.,-1.));
#6630=DIRECTION('center_axis',(-4.28708778888548E-14,3.11475159991785E-14,
1.));
#6631=DIRECTION('ref_axis',(1.,1.47528330277905E-31,4.28708778888548E-14));
#6632=DIRECTION('',(0.,0.,1.));
#6633=DIRECTION('center_axis',(0.,0.,-1.));
#6634=DIRECTION('ref_axis',(-1.,0.,0.));
#6635=DIRECTION('center_axis',(-3.5458113632178E-14,3.93802247521331E-14,
1.));
#6636=DIRECTION('ref_axis',(8.56410063824163E-32,-1.,3.93802247521331E-14));
#6637=DIRECTION('',(0.,0.,1.));
#6638=DIRECTION('center_axis',(3.54581136321754E-14,-3.93802247521304E-14,
1.));
#6639=DIRECTION('ref_axis',(8.56410065781048E-32,-1.,-3.93802247521304E-14));
#6640=DIRECTION('',(0.,0.,-1.));
#6641=DIRECTION('center_axis',(0.,0.,-1.));
#6642=DIRECTION('ref_axis',(-1.,0.,0.));
#6643=DIRECTION('center_axis',(4.84099790644884E-14,-2.15535113346964E-14,
1.));
#6644=DIRECTION('ref_axis',(1.,5.08629419547381E-32,-4.84099790644884E-14));
#6645=DIRECTION('',(0.,0.,-1.));
#6646=DIRECTION('center_axis',(-4.84099790644954E-14,2.15535113347002E-14,
1.));
#6647=DIRECTION('ref_axis',(1.,5.08629422365244E-32,4.84099790644954E-14));
#6648=DIRECTION('',(0.,0.,1.));
#6649=DIRECTION('center_axis',(0.,0.,-1.));
#6650=DIRECTION('ref_axis',(-1.,0.,0.));
#6651=DIRECTION('center_axis',(5.1833331858162E-14,-1.10175147996729E-14,
1.));
#6652=DIRECTION('ref_axis',(1.,2.6934165387896E-32,-5.1833331858162E-14));
#6653=DIRECTION('',(0.,0.,-1.));
#6654=DIRECTION('center_axis',(-5.18333318581728E-14,1.1017514799675E-14,
1.));
#6655=DIRECTION('ref_axis',(1.,2.69341656191485E-32,5.18333318581728E-14));
#6656=DIRECTION('',(0.,0.,1.));
#6657=DIRECTION('center_axis',(0.,0.,-1.));
#6658=DIRECTION('ref_axis',(1.,-1.00915871466367E-14,0.));
#6659=DIRECTION('center_axis',(5.29913193257013E-14,-5.35591413351499E-28,
1.));
#6660=DIRECTION('ref_axis',(1.,-2.18591407531132E-45,-5.29913193257013E-14));
#6661=DIRECTION('',(0.,0.,-1.));
#6662=DIRECTION('center_axis',(-5.29913193257013E-14,5.35591413351499E-28,
1.));
#6663=DIRECTION('ref_axis',(1.,-2.18591407531132E-45,5.29913193257013E-14));
#6664=DIRECTION('',(0.,0.,1.));
#6665=DIRECTION('center_axis',(0.,0.,-1.));
#6666=DIRECTION('ref_axis',(-1.,0.,0.));
#6667=DIRECTION('center_axis',(5.18333318581513E-14,1.10175147996694E-14,
1.));
#6668=DIRECTION('ref_axis',(1.,-2.69341651343199E-32,-5.18333318581513E-14));
#6669=DIRECTION('',(0.,0.,-1.));
#6670=DIRECTION('center_axis',(-5.18333318581518E-14,-1.10175147996696E-14,
1.));
#6671=DIRECTION('ref_axis',(1.,-2.69341651413071E-32,5.18333318581518E-14));
#6672=DIRECTION('',(0.,0.,1.));
#6673=DIRECTION('center_axis',(0.,0.,-1.));
#6674=DIRECTION('ref_axis',(-1.,0.,0.));
#6675=DIRECTION('center_axis',(3.54581136321655E-14,3.93802247521174E-14,
1.));
#6676=DIRECTION('ref_axis',(-8.56410074679405E-32,-1.,3.93802247521174E-14));
#6677=DIRECTION('',(0.,0.,-1.));
#6678=DIRECTION('center_axis',(-3.54581136321788E-14,-3.93802247521323E-14,
1.));
#6679=DIRECTION('ref_axis',(-8.56410064023259E-32,-1.,-3.93802247521323E-14));
#6680=DIRECTION('',(0.,0.,1.));
#6681=DIRECTION('center_axis',(0.,0.,-1.));
#6682=DIRECTION('ref_axis',(-1.,0.,0.));
#6683=DIRECTION('center_axis',(-2.64956596628558E-14,-4.58918287161185E-14,
1.));
#6684=DIRECTION('ref_axis',(1.05337643492684E-31,-1.,-4.58918287161185E-14));
#6685=DIRECTION('',(0.,0.,1.));
#6686=DIRECTION('center_axis',(2.64956596628559E-14,4.58918287161184E-14,
1.));
#6687=DIRECTION('ref_axis',(1.05337643521562E-31,-1.,4.58918287161184E-14));
#6688=DIRECTION('',(0.,0.,-1.));
#6689=DIRECTION('center_axis',(0.,0.,-1.));
#6690=DIRECTION('ref_axis',(-1.,0.,0.));
#6691=DIRECTION('center_axis',(-4.28708778888579E-14,-3.114751599918E-14,
1.));
#6692=DIRECTION('ref_axis',(1.,-1.47528330530812E-31,4.28708778888579E-14));
#6693=DIRECTION('',(0.,0.,1.));
#6694=DIRECTION('center_axis',(4.28708778888557E-14,3.11475159991785E-14,
1.));
#6695=DIRECTION('ref_axis',(1.,-1.47528330426136E-31,-4.28708778888557E-14));
#6696=DIRECTION('',(0.,0.,-1.));
#6697=DIRECTION('center_axis',(0.,0.,-1.));
#6698=DIRECTION('ref_axis',(-1.,0.,0.));
#6699=DIRECTION('center_axis',(-4.8409979064494E-14,-2.15535113346981E-14,
1.));
#6700=DIRECTION('ref_axis',(1.,-5.0862942118997E-32,4.8409979064494E-14));
#6701=DIRECTION('',(0.,0.,1.));
#6702=DIRECTION('center_axis',(4.84099790644959E-14,2.15535113346995E-14,
1.));
#6703=DIRECTION('ref_axis',(1.,-5.08629422237696E-32,-4.84099790644959E-14));
#6704=DIRECTION('',(0.,0.,-1.));
#6705=DIRECTION('center_axis',(0.,0.,-1.));
#6706=DIRECTION('ref_axis',(-1.,0.,0.));
#6707=DIRECTION('center_axis',(-5.53910117564113E-15,-5.27010273338631E-14,
1.));
#6708=DIRECTION('ref_axis',(-1.7974049544022E-32,-1.,-5.27010273338631E-14));
#6709=DIRECTION('',(0.,0.,-1.));
#6710=DIRECTION('center_axis',(5.53910117564113E-15,5.27010273338631E-14,
1.));
#6711=DIRECTION('ref_axis',(-1.7974049544022E-32,-1.,5.27010273338631E-14));
#6712=DIRECTION('',(0.,0.,1.));
#6713=DIRECTION('center_axis',(0.,0.,1.));
#6714=DIRECTION('ref_axis',(1.,0.,0.));
#6715=DIRECTION('center_axis',(-1.60923747916482E-15,8.29484928207641E-16,
-1.));
#6716=DIRECTION('ref_axis',(-1.,-1.60052481612529E-33,1.60923747916482E-15));
#6717=DIRECTION('center_axis',(0.,0.,1.));
#6718=DIRECTION('ref_axis',(1.,0.,0.));
#6719=DIRECTION('center_axis',(0.,0.,-1.));
#6720=DIRECTION('ref_axis',(-1.,0.,0.));
#6721=DIRECTION('center_axis',(0.,0.,1.));
#6722=DIRECTION('ref_axis',(1.,0.,0.));
#6723=DIRECTION('center_axis',(0.,0.,-1.));
#6724=DIRECTION('ref_axis',(-1.,0.,0.));
#6725=DIRECTION('center_axis',(-7.00806082662238E-16,5.72968988795807E-16,
-1.));
#6726=DIRECTION('ref_axis',(-1.,2.77391763959705E-33,7.00806082662238E-16));
#6727=DIRECTION('center_axis',(0.,0.,1.));
#6728=DIRECTION('ref_axis',(1.,0.,0.));
#6729=DIRECTION('center_axis',(0.,0.,-1.));
#6730=DIRECTION('ref_axis',(-1.,0.,0.));
#6731=DIRECTION('center_axis',(4.63562821373925E-16,1.3774000978861E-15,
1.));
#6732=DIRECTION('ref_axis',(-1.06074921525595E-31,-1.,1.3774000978861E-15));
#6733=DIRECTION('center_axis',(2.9160531709346E-16,-1.78680073022012E-15,
-1.));
#6734=DIRECTION('ref_axis',(-4.81742820615547E-33,1.,-1.78680073022012E-15));
#6735=DIRECTION('center_axis',(-5.66364837089041E-16,7.06154019267167E-16,
-1.));
#6736=DIRECTION('ref_axis',(2.86938317203061E-34,1.,7.06154019267168E-16));
#6737=DIRECTION('center_axis',(0.,0.,1.));
#6738=DIRECTION('ref_axis',(1.,0.,0.));
#6739=DIRECTION('center_axis',(0.,0.,-1.));
#6740=DIRECTION('ref_axis',(-1.,0.,0.));
#6741=DIRECTION('center_axis',(0.,0.,1.));
#6742=DIRECTION('ref_axis',(1.,0.,0.));
#6743=DIRECTION('center_axis',(-4.31318598491438E-17,-9.04191500891283E-16,
-1.));
#6744=DIRECTION('ref_axis',(-1.09164579339903E-34,1.,-9.04191500891283E-16));
#6745=DIRECTION('center_axis',(0.,0.,-1.));
#6746=DIRECTION('ref_axis',(-1.,0.,0.));
#6747=DIRECTION('center_axis',(1.18464566449553E-15,-8.41864697328891E-16,
1.));
#6748=DIRECTION('ref_axis',(1.,9.58283674537864E-32,-1.18464566449553E-15));
#6749=DIRECTION('center_axis',(0.,0.,-1.));
#6750=DIRECTION('ref_axis',(-1.,0.,0.));
#6751=DIRECTION('center_axis',(9.83724801784613E-16,1.06976961695994E-15,
1.));
#6752=DIRECTION('ref_axis',(-1.03029779618179E-33,-1.,1.06976961695994E-15));
#6753=DIRECTION('center_axis',(-2.3018130899998E-16,-8.75465129291354E-16,
-1.));
#6754=DIRECTION('ref_axis',(-2.99401685848927E-33,1.,-8.75465129291354E-16));
#6755=DIRECTION('center_axis',(0.,0.,-1.));
#6756=DIRECTION('ref_axis',(-1.,0.,0.));
#6757=DIRECTION('center_axis',(0.,0.,1.));
#6758=DIRECTION('ref_axis',(1.,0.,0.));
#6759=DIRECTION('center_axis',(0.,0.,-1.));
#6760=DIRECTION('ref_axis',(-1.,0.,0.));
#6761=DIRECTION('center_axis',(0.,0.,1.));
#6762=DIRECTION('ref_axis',(1.,0.,0.));
#6763=DIRECTION('center_axis',(-8.14341460830106E-16,-1.61695346118725E-15,
-1.));
#6764=DIRECTION('ref_axis',(-7.85474895342403E-33,1.,-1.61695346118725E-15));
#6765=DIRECTION('center_axis',(-8.62637196982729E-17,1.80838300178258E-15,
-1.));
#6766=DIRECTION('ref_axis',(4.36658317362438E-34,1.,1.80838300178258E-15));
#6767=DIRECTION('center_axis',(0.,0.,1.));
#6768=DIRECTION('ref_axis',(1.,0.,0.));
#6769=DIRECTION('center_axis',(0.,0.,-1.));
#6770=DIRECTION('ref_axis',(-1.,0.,0.));
#6771=DIRECTION('center_axis',(0.,0.,1.));
#6772=DIRECTION('ref_axis',(1.,0.,0.));
#6773=DIRECTION('center_axis',(-1.1327296741781E-15,-1.41230803853433E-15,
-1.));
#6774=DIRECTION('ref_axis',(-1.14775326881119E-33,1.,-1.41230803853433E-15));
#6775=DIRECTION('center_axis',(2.91605317093473E-16,1.78680073022013E-15,
-1.));
#6776=DIRECTION('ref_axis',(4.81742820615223E-33,1.,1.78680073022013E-15));
#6777=DIRECTION('center_axis',(0.,0.,1.));
#6778=DIRECTION('ref_axis',(1.,0.,0.));
#6779=DIRECTION('center_axis',(0.,0.,-1.));
#6780=DIRECTION('ref_axis',(-1.,0.,0.));
#6781=DIRECTION('center_axis',(0.,0.,1.));
#6782=DIRECTION('ref_axis',(1.,0.,0.));
#6783=DIRECTION('center_axis',(-7.00806082662235E-16,-5.72968988795798E-16,
-1.));
#6784=DIRECTION('ref_axis',(-1.,-2.77391763959813E-33,7.00806082662235E-16));
#6785=DIRECTION('center_axis',(6.5672980225067E-16,1.68712669272586E-15,
-1.));
#6786=DIRECTION('ref_axis',(-9.28280238043588E-34,1.,1.68712669272585E-15));
#6787=DIRECTION('center_axis',(0.,0.,1.));
#6788=DIRECTION('ref_axis',(1.,0.,0.));
#6789=DIRECTION('center_axis',(0.,0.,-1.));
#6790=DIRECTION('ref_axis',(-1.,0.,0.));
#6791=DIRECTION('center_axis',(1.45323412840514E-15,-1.52344036793355E-17,
1.));
#6792=DIRECTION('ref_axis',(1.,-2.33073141122416E-33,-1.45323412840514E-15));
#6793=DIRECTION('center_axis',(-8.04618739582399E-16,-4.14742464103809E-16,
-1.));
#6794=DIRECTION('ref_axis',(-1.,-7.72936702803813E-33,8.04618739582399E-16));
#6795=DIRECTION('center_axis',(9.93152043710288E-16,1.51371712302743E-15,
-1.));
#6796=DIRECTION('ref_axis',(1.50815602913674E-32,1.,1.51371712302743E-15));
#6797=DIRECTION('center_axis',(1.3675338218833E-16,1.44686558860067E-15,
1.));
#6798=DIRECTION('ref_axis',(-2.17929987622515E-32,-1.,1.44686558860067E-15));
#6799=DIRECTION('center_axis',(0.,0.,-1.));
#6800=DIRECTION('ref_axis',(-1.,0.,0.));
#6801=DIRECTION('center_axis',(0.,0.,1.));
#6802=DIRECTION('ref_axis',(1.,0.,0.));
#6803=DIRECTION('center_axis',(-8.73265696593734E-16,-2.38389703575337E-16,
-1.));
#6804=DIRECTION('ref_axis',(-1.,2.57646307002847E-33,8.73265696593734E-16));
#6805=DIRECTION('center_axis',(1.28616877518753E-15,1.27415085143204E-15,
-1.));
#6806=DIRECTION('ref_axis',(-1.,-9.57919634854104E-33,-1.28616877518753E-15));
#6807=DIRECTION('center_axis',(0.,0.,1.));
#6808=DIRECTION('ref_axis',(1.,0.,0.));
#6809=DIRECTION('center_axis',(0.,0.,-1.));
#6810=DIRECTION('ref_axis',(-1.,0.,0.));
#6811=DIRECTION('center_axis',(0.,0.,1.));
#6812=DIRECTION('ref_axis',(1.,0.,0.));
#6813=DIRECTION('center_axis',(0.,0.,-1.));
#6814=DIRECTION('ref_axis',(-1.,0.,0.));
#6815=DIRECTION('center_axis',(0.,0.,-1.));
#6816=DIRECTION('ref_axis',(-1.,0.,0.));
#6817=DIRECTION('center_axis',(0.,0.,1.));
#6818=DIRECTION('ref_axis',(1.,0.,0.));
#6819=DIRECTION('center_axis',(0.,0.,-1.));
#6820=DIRECTION('ref_axis',(-1.,0.,0.));
#6821=DIRECTION('center_axis',(0.,0.,1.));
#6822=DIRECTION('ref_axis',(1.,0.,0.));
#6823=DIRECTION('center_axis',(-8.94729738214378E-16,1.37409327095771E-16,
-1.));
#6824=DIRECTION('ref_axis',(-1.,9.52358310446502E-34,8.94729738214378E-16));
#6825=DIRECTION('center_axis',(1.69321748241794E-15,6.40862752628506E-16,
-1.));
#6826=DIRECTION('ref_axis',(-1.,4.80921258843877E-33,-1.69321748241794E-15));
#6827=DIRECTION('center_axis',(0.,0.,1.));
#6828=DIRECTION('ref_axis',(1.,0.,0.));
#6829=DIRECTION('center_axis',(0.,0.,-1.));
#6830=DIRECTION('ref_axis',(-1.,0.,0.));
#6831=DIRECTION('center_axis',(0.,0.,1.));
#6832=DIRECTION('ref_axis',(1.,0.,0.));
#6833=DIRECTION('center_axis',(-1.69321748241794E-15,6.40862752628506E-16,
-1.));
#6834=DIRECTION('ref_axis',(-1.,-4.80921258844117E-33,1.69321748241794E-15));
#6835=DIRECTION('center_axis',(0.,0.,-1.));
#6836=DIRECTION('ref_axis',(-1.,0.,0.));
#6837=DIRECTION('center_axis',(0.,0.,1.));
#6838=DIRECTION('ref_axis',(1.,0.,0.));
#6839=DIRECTION('center_axis',(-7.61486879733257E-16,4.89449036787473E-16,
-1.));
#6840=DIRECTION('ref_axis',(-1.,-8.14289481143214E-33,7.61486879733257E-16));
#6841=DIRECTION('center_axis',(0.,0.,-1.));
#6842=DIRECTION('ref_axis',(-1.,0.,0.));
#6843=DIRECTION('center_axis',(0.,0.,1.));
#6844=DIRECTION('ref_axis',(1.,0.,0.));
#6845=DIRECTION('center_axis',(-6.43084387593755E-16,6.37075425716024E-16,
-1.));
#6846=DIRECTION('ref_axis',(-1.,-1.00927178548204E-32,6.43084387593755E-16));
#6847=DIRECTION('center_axis',(1.74653139318747E-15,-4.76779407150702E-16,
-1.));
#6848=DIRECTION('ref_axis',(-1.,8.38515567293037E-33,-1.74653139318747E-15));
#6849=DIRECTION('center_axis',(0.,0.,-1.));
#6850=DIRECTION('ref_axis',(-1.,0.,0.));
#6851=DIRECTION('center_axis',(0.,0.,1.));
#6852=DIRECTION('ref_axis',(1.,0.,0.));
#6853=DIRECTION('center_axis',(0.,0.,-1.));
#6854=DIRECTION('ref_axis',(-1.,0.,0.));
#6855=DIRECTION('center_axis',(8.04618739582395E-16,-4.14742464103823E-16,
-1.));
#6856=DIRECTION('ref_axis',(-1.,7.72936702804043E-33,-8.04618739582395E-16));
#6857=DIRECTION('center_axis',(0.,0.,-1.));
#6858=DIRECTION('ref_axis',(-1.,0.,0.));
#6859=DIRECTION('center_axis',(0.,0.,1.));
#6860=DIRECTION('ref_axis',(1.,0.,0.));
#6861=DIRECTION('center_axis',(0.,0.,-1.));
#6862=DIRECTION('ref_axis',(-1.,0.,0.));
#6863=DIRECTION('center_axis',(1.40161216532447E-15,-1.14593797759163E-15,
-1.));
#6864=DIRECTION('ref_axis',(-1.,1.10956705583757E-32,-1.40161216532447E-15));
#6865=DIRECTION('center_axis',(0.,0.,-1.));
#6866=DIRECTION('ref_axis',(-1.,0.,0.));
#6867=DIRECTION('center_axis',(0.,0.,1.));
#6868=DIRECTION('ref_axis',(1.,0.,0.));
#6869=DIRECTION('center_axis',(-2.91605317093444E-16,1.78680073022012E-15,
-1.));
#6870=DIRECTION('ref_axis',(-4.81742820615669E-33,1.,1.78680073022012E-15));
#6871=DIRECTION('center_axis',(0.,0.,-1.));
#6872=DIRECTION('ref_axis',(-1.,0.,0.));
#6873=DIRECTION('center_axis',(0.,0.,-1.));
#6874=DIRECTION('ref_axis',(-1.,0.,0.));
#6875=DIRECTION('center_axis',(-7.39810444800344E-16,-1.25092047100568E-15,
1.));
#6876=DIRECTION('ref_axis',(1.33242458232468E-31,-1.,-1.25092047100568E-15));
#6877=DIRECTION('center_axis',(4.31318598491496E-17,9.04191500891285E-16,
-1.));
#6878=DIRECTION('ref_axis',(-1.09164579339958E-34,1.,9.04191500891285E-16));
#6879=DIRECTION('center_axis',(4.07170730415042E-16,-8.08476730593626E-16,
-1.));
#6880=DIRECTION('ref_axis',(-6.01739504654964E-33,1.,-8.08476730593626E-16));
#6881=DIRECTION('center_axis',(0.,0.,-1.));
#6882=DIRECTION('ref_axis',(-1.,0.,0.));
#6883=DIRECTION('center_axis',(0.,0.,1.));
#6884=DIRECTION('ref_axis',(1.,0.,0.));
#6885=DIRECTION('center_axis',(2.30181308999987E-16,8.75465129291357E-16,
-1.));
#6886=DIRECTION('ref_axis',(-2.99401685849059E-33,1.,8.75465129291357E-16));
#6887=DIRECTION('center_axis',(2.3018130899997E-16,-8.75465129291361E-16,
-1.));
#6888=DIRECTION('ref_axis',(2.99401685849076E-33,1.,-8.75465129291361E-16));
#6889=DIRECTION('center_axis',(0.,0.,1.));
#6890=DIRECTION('ref_axis',(1.,0.,0.));
#6891=DIRECTION('center_axis',(0.,0.,-1.));
#6892=DIRECTION('ref_axis',(-1.,0.,0.));
#6893=DIRECTION('center_axis',(0.,0.,-1.));
#6894=DIRECTION('ref_axis',(-1.,0.,0.));
#6895=DIRECTION('center_axis',(8.62637196982607E-17,-1.80838300178258E-15,
-1.));
#6896=DIRECTION('ref_axis',(4.36658317360467E-34,1.,-1.80838300178258E-15));
#6897=DIRECTION('center_axis',(0.,0.,1.));
#6898=DIRECTION('ref_axis',(1.,0.,0.));
#6899=DIRECTION('center_axis',(0.,0.,-1.));
#6900=DIRECTION('ref_axis',(-1.,0.,0.));
#6901=DIRECTION('center_axis',(1.13272967417811E-15,1.41230803853433E-15,
-1.));
#6902=DIRECTION('ref_axis',(-1.1477532688217E-33,1.,1.41230803853433E-15));
#6903=DIRECTION('center_axis',(-1.4580265854674E-16,-8.93400365110051E-16,
-1.));
#6904=DIRECTION('ref_axis',(1.20435705154195E-33,1.,-8.9340036511005E-16));
#6905=DIRECTION('center_axis',(0.,0.,1.));
#6906=DIRECTION('ref_axis',(1.,0.,0.));
#6907=DIRECTION('center_axis',(0.,0.,-1.));
#6908=DIRECTION('ref_axis',(-1.,0.,0.));
#6909=DIRECTION('center_axis',(7.00806082662235E-16,5.7296898879579E-16,
-1.));
#6910=DIRECTION('ref_axis',(-1.,-2.77391763960031E-33,-7.00806082662235E-16));
#6911=DIRECTION('center_axis',(-6.5672980225068E-16,-1.68712669272586E-15,
-1.));
#6912=DIRECTION('ref_axis',(-9.28280238055324E-34,1.,-1.68712669272586E-15));
#6913=DIRECTION('center_axis',(0.,0.,1.));
#6914=DIRECTION('ref_axis',(1.,0.,0.));
#6915=DIRECTION('center_axis',(0.,0.,-1.));
#6916=DIRECTION('ref_axis',(-1.,0.,0.));
#6917=DIRECTION('center_axis',(0.,0.,-1.));
#6918=DIRECTION('ref_axis',(-1.,0.,0.));
#6919=DIRECTION('center_axis',(-9.93152043710293E-16,-1.51371712302739E-15,
-1.));
#6920=DIRECTION('ref_axis',(1.50815602914153E-32,1.,-1.51371712302739E-15));
#6921=DIRECTION('center_axis',(0.,0.,1.));
#6922=DIRECTION('ref_axis',(1.,0.,0.));
#6923=DIRECTION('center_axis',(0.,0.,-1.));
#6924=DIRECTION('ref_axis',(-1.,0.,0.));
#6925=DIRECTION('center_axis',(8.73265696593737E-16,2.38389703575328E-16,
-1.));
#6926=DIRECTION('ref_axis',(-1.,2.57646307002799E-33,-8.73265696593737E-16));
#6927=DIRECTION('center_axis',(-6.43084387593757E-16,-6.37075425716002E-16,
-1.));
#6928=DIRECTION('ref_axis',(-1.,1.00927178548153E-32,6.43084387593757E-16));
#6929=DIRECTION('center_axis',(0.,0.,1.));
#6930=DIRECTION('ref_axis',(1.,0.,0.));
#6931=DIRECTION('center_axis',(0.,0.,-1.));
#6932=DIRECTION('ref_axis',(-1.,0.,0.));
#6933=DIRECTION('center_axis',(-1.52297375946654E-15,-9.78898073574922E-16,
-1.));
#6934=DIRECTION('ref_axis',(-1.,-5.80380233320457E-33,1.52297375946654E-15));
#6935=DIRECTION('center_axis',(0.,0.,1.));
#6936=DIRECTION('ref_axis',(1.,0.,0.));
#6937=DIRECTION('center_axis',(0.,0.,-1.));
#6938=DIRECTION('ref_axis',(-1.,0.,0.));
#6939=DIRECTION('center_axis',(-5.53910117564523E-15,5.27010273339079E-14,
1.));
#6940=DIRECTION('ref_axis',(1.79740492095489E-32,-1.,5.27010273339079E-14));
#6941=DIRECTION('center_axis',(-8.46608741208968E-16,-3.20431376314253E-16,
-1.));
#6942=DIRECTION('ref_axis',(-1.,-5.07857362029075E-33,8.46608741208968E-16));
#6943=DIRECTION('center_axis',(0.,0.,1.));
#6944=DIRECTION('ref_axis',(1.,0.,0.));
#6945=DIRECTION('center_axis',(0.,0.,-1.));
#6946=DIRECTION('ref_axis',(-1.,0.,0.));
#6947=DIRECTION('center_axis',(0.,0.,1.));
#6948=DIRECTION('ref_axis',(1.,0.,0.));
#6949=DIRECTION('center_axis',(8.46608741208968E-16,-3.20431376314254E-16,
-1.));
#6950=DIRECTION('ref_axis',(-1.,5.07857362029218E-33,-8.46608741208968E-16));
#6951=DIRECTION('center_axis',(-8.94729738214377E-16,-1.37409327095765E-16,
-1.));
#6952=DIRECTION('ref_axis',(-1.,-9.52358310446232E-34,8.94729738214377E-16));
#6953=DIRECTION('center_axis',(0.,0.,1.));
#6954=DIRECTION('ref_axis',(1.,0.,0.));
#6955=DIRECTION('center_axis',(0.,0.,-1.));
#6956=DIRECTION('ref_axis',(-1.,0.,0.));
#6957=DIRECTION('center_axis',(0.,0.,1.));
#6958=DIRECTION('ref_axis',(1.,0.,0.));
#6959=DIRECTION('center_axis',(7.61486879733261E-16,-4.89449036787468E-16,
-1.));
#6960=DIRECTION('ref_axis',(-1.,-8.14289481143569E-33,-7.61486879733261E-16));
#6961=DIRECTION('center_axis',(-9.03746752270189E-16,5.16181690799129E-17,
-1.));
#6962=DIRECTION('ref_axis',(-1.,-1.07685893901366E-34,9.03746752270189E-16));
#6963=DIRECTION('center_axis',(0.,0.,1.));
#6964=DIRECTION('ref_axis',(1.,0.,0.));
#6965=DIRECTION('center_axis',(0.,0.,-1.));
#6966=DIRECTION('ref_axis',(-1.,0.,0.));
#6967=DIRECTION('center_axis',(-4.34585263591718E-16,1.38681547715823E-15,
1.));
#6968=DIRECTION('ref_axis',(9.53523368488341E-32,-1.,1.38681547715823E-15));
#6969=DIRECTION('center_axis',(0.,0.,-1.));
#6970=DIRECTION('ref_axis',(-1.,0.,0.));
#6971=DIRECTION('center_axis',(0.,0.,-1.));
#6972=DIRECTION('ref_axis',(-1.,0.,0.));
#6973=DIRECTION('center_axis',(0.,0.,1.));
#6974=DIRECTION('ref_axis',(1.,0.,0.));
#6975=DIRECTION('center_axis',(0.,0.,-1.));
#6976=DIRECTION('ref_axis',(-1.,0.,0.));
#6977=DIRECTION('center_axis',(-1.36753382188316E-16,1.44686558860067E-15,
1.));
#6978=DIRECTION('ref_axis',(2.17929987622488E-32,-1.,1.44686558860067E-15));
#6979=DIRECTION('center_axis',(4.96576021855139E-16,-7.5685856151371E-16,
-1.));
#6980=DIRECTION('ref_axis',(5.96315361064996E-33,1.,-7.5685856151371E-16));
#6981=DIRECTION('',(-1.,0.,0.));
#6982=DIRECTION('',(1.13134139737618E-16,-1.,0.));
#6983=DIRECTION('',(1.13134139737618E-16,1.,0.));
#6984=DIRECTION('center_axis',(0.,0.,1.));
#6985=DIRECTION('ref_axis',(1.,0.,0.));
#6986=DIRECTION('center_axis',(1.60923747916481E-15,-8.29484928207644E-16,
-1.));
#6987=DIRECTION('ref_axis',(-1.,-1.60052481610948E-33,-1.60923747916481E-15));
#6988=DIRECTION('center_axis',(-9.93152043710277E-16,1.51371712302743E-15,
-1.));
#6989=DIRECTION('ref_axis',(-1.50815602913694E-32,1.,1.51371712302743E-15));
#6990=DIRECTION('center_axis',(-1.36753382188316E-16,1.44686558860067E-15,
-1.));
#6991=DIRECTION('ref_axis',(-2.17929987622498E-32,1.,1.44686558860067E-15));
#6992=DIRECTION('center_axis',(0.,0.,-1.));
#6993=DIRECTION('ref_axis',(-1.,0.,0.));
#6994=DIRECTION('center_axis',(0.,0.,-1.));
#6995=DIRECTION('ref_axis',(-1.,0.,0.));
#6996=DIRECTION('center_axis',(8.73265696593735E-16,-2.38389703575344E-16,
-1.));
#6997=DIRECTION('ref_axis',(-1.,-2.57646307002882E-33,-8.73265696593735E-16));
#6998=DIRECTION('center_axis',(0.,0.,-1.));
#6999=DIRECTION('ref_axis',(-1.,0.,0.));
#7000=DIRECTION('center_axis',(-4.34585263591734E-16,1.38681547715824E-15,
-1.));
#7001=DIRECTION('ref_axis',(-9.53523368488213E-32,1.,1.38681547715824E-15));
#7002=DIRECTION('center_axis',(0.,0.,-1.));
#7003=DIRECTION('ref_axis',(-1.,0.,0.));
#7004=DIRECTION('center_axis',(0.,0.,-1.));
#7005=DIRECTION('ref_axis',(-1.,0.,0.));
#7006=DIRECTION('center_axis',(0.,0.,-1.));
#7007=DIRECTION('ref_axis',(-1.,0.,0.));
#7008=DIRECTION('center_axis',(-1.52297375946653E-15,9.78898073574935E-16,
-1.));
#7009=DIRECTION('ref_axis',(-1.,5.80380233323614E-33,1.52297375946653E-15));
#7010=DIRECTION('center_axis',(0.,0.,-1.));
#7011=DIRECTION('ref_axis',(-1.,0.,0.));
#7012=DIRECTION('center_axis',(0.,0.,-1.));
#7013=DIRECTION('ref_axis',(-1.,0.,0.));
#7014=DIRECTION('center_axis',(0.,0.,-1.));
#7015=DIRECTION('ref_axis',(-1.,0.,0.));
#7016=DIRECTION('center_axis',(8.9472973821438E-16,1.37409327095766E-16,
-1.));
#7017=DIRECTION('ref_axis',(-1.,-9.52358310444862E-34,-8.94729738214381E-16));
#7018=DIRECTION('center_axis',(-8.4660874120897E-16,3.20431376314254E-16,
-1.));
#7019=DIRECTION('ref_axis',(-1.,5.07857362028999E-33,8.4660874120897E-16));
#7020=DIRECTION('center_axis',(0.,0.,-1.));
#7021=DIRECTION('ref_axis',(-1.,0.,0.));
#7022=DIRECTION('center_axis',(0.,0.,-1.));
#7023=DIRECTION('ref_axis',(-1.,0.,0.));
#7024=DIRECTION('center_axis',(0.,0.,-1.));
#7025=DIRECTION('ref_axis',(-1.,0.,0.));
#7026=DIRECTION('center_axis',(0.,0.,-1.));
#7027=DIRECTION('ref_axis',(-1.,0.,0.));
#7028=DIRECTION('center_axis',(5.53910117564333E-15,-5.27010273338855E-14,
1.));
#7029=DIRECTION('ref_axis',(1.79740494482853E-32,-1.,-5.27010273338855E-14));
#7030=DIRECTION('center_axis',(0.,0.,-1.));
#7031=DIRECTION('ref_axis',(-1.,0.,0.));
#7032=DIRECTION('center_axis',(0.,0.,-1.));
#7033=DIRECTION('ref_axis',(-1.,0.,0.));
#7034=DIRECTION('center_axis',(7.61486879733267E-16,4.89449036787458E-16,
-1.));
#7035=DIRECTION('ref_axis',(-1.,8.14289481143805E-33,-7.61486879733267E-16));
#7036=DIRECTION('center_axis',(0.,0.,-1.));
#7037=DIRECTION('ref_axis',(-1.,0.,0.));
#7038=DIRECTION('center_axis',(4.34585263591789E-16,1.38681547715822E-15,
-1.));
#7039=DIRECTION('ref_axis',(9.53523368488375E-32,1.,1.38681547715822E-15));
#7040=DIRECTION('center_axis',(6.43084387593757E-16,6.37075425716005E-16,
-1.));
#7041=DIRECTION('ref_axis',(-1.,1.00927178548155E-32,-6.43084387593758E-16));
#7042=DIRECTION('center_axis',(-8.73265696593747E-16,-2.38389703575334E-16,
-1.));
#7043=DIRECTION('ref_axis',(-1.,2.57646307003222E-33,8.73265696593746E-16));
#7044=DIRECTION('center_axis',(0.,0.,-1.));
#7045=DIRECTION('ref_axis',(-1.,0.,0.));
#7046=DIRECTION('center_axis',(0.,0.,-1.));
#7047=DIRECTION('ref_axis',(-1.,0.,0.));
#7048=DIRECTION('center_axis',(4.96576021855147E-16,7.568585615137E-16,
-1.));
#7049=DIRECTION('ref_axis',(-5.96315361064353E-33,1.,7.568585615137E-16));
#7050=DIRECTION('center_axis',(0.,0.,-1.));
#7051=DIRECTION('ref_axis',(-1.,0.,0.));
#7052=DIRECTION('center_axis',(0.,0.,-1.));
#7053=DIRECTION('ref_axis',(-1.,0.,0.));
#7054=DIRECTION('center_axis',(0.,0.,-1.));
#7055=DIRECTION('ref_axis',(-1.,0.,0.));
#7056=DIRECTION('center_axis',(6.56729802250692E-16,1.68712669272589E-15,
-1.));
#7057=DIRECTION('ref_axis',(-9.28280238086152E-34,1.,1.68712669272589E-15));
#7058=DIRECTION('center_axis',(-7.00806082662247E-16,-5.72968988795798E-16,
-1.));
#7059=DIRECTION('ref_axis',(-1.,-2.77391763959015E-33,7.00806082662247E-16));
#7060=DIRECTION('center_axis',(0.,0.,-1.));
#7061=DIRECTION('ref_axis',(-1.,0.,0.));
#7062=DIRECTION('center_axis',(0.,0.,-1.));
#7063=DIRECTION('ref_axis',(-1.,0.,0.));
#7064=DIRECTION('center_axis',(1.45802658546741E-16,8.93400365110057E-16,
-1.));
#7065=DIRECTION('ref_axis',(1.20435705154029E-33,1.,8.93400365110057E-16));
#7066=DIRECTION('center_axis',(-5.66364837089057E-16,-7.06154019267168E-16,
-1.));
#7067=DIRECTION('ref_axis',(-2.8693831720744E-34,1.,-7.06154019267168E-16));
#7068=DIRECTION('center_axis',(0.,0.,-1.));
#7069=DIRECTION('ref_axis',(-1.,0.,0.));
#7070=DIRECTION('center_axis',(0.,0.,-1.));
#7071=DIRECTION('ref_axis',(-1.,0.,0.));
#7072=DIRECTION('center_axis',(-8.62637196982615E-17,1.80838300178258E-15,
-1.));
#7073=DIRECTION('ref_axis',(4.3665831736119E-34,1.,1.80838300178258E-15));
#7074=DIRECTION('center_axis',(-8.14341460830121E-16,-1.61695346118725E-15,
-1.));
#7075=DIRECTION('ref_axis',(-7.85474895342543E-33,1.,-1.61695346118725E-15));
#7076=DIRECTION('center_axis',(0.,0.,-1.));
#7077=DIRECTION('ref_axis',(-1.,0.,0.));
#7078=DIRECTION('center_axis',(0.,0.,-1.));
#7079=DIRECTION('ref_axis',(-1.,0.,0.));
#7080=DIRECTION('center_axis',(-2.3018130899997E-16,8.75465129291364E-16,
-1.));
#7081=DIRECTION('ref_axis',(2.9940168584926E-33,1.,8.75465129291364E-16));
#7082=DIRECTION('center_axis',(-2.30181308999987E-16,-8.75465129291357E-16,
-1.));
#7083=DIRECTION('ref_axis',(-2.99401685849059E-33,1.,-8.75465129291357E-16));
#7084=DIRECTION('center_axis',(0.,0.,-1.));
#7085=DIRECTION('ref_axis',(-1.,0.,0.));
#7086=DIRECTION('center_axis',(0.,0.,-1.));
#7087=DIRECTION('ref_axis',(-1.,0.,0.));
#7088=DIRECTION('center_axis',(-4.07170730415043E-16,8.08476730593629E-16,
-1.));
#7089=DIRECTION('ref_axis',(-6.01739504654846E-33,1.,8.08476730593629E-16));
#7090=DIRECTION('center_axis',(-4.31318598491494E-17,-9.04191500891281E-16,
-1.));
#7091=DIRECTION('ref_axis',(-1.09164579339739E-34,1.,-9.04191500891281E-16));
#7092=DIRECTION('center_axis',(-7.39810444800352E-16,-1.25092047100568E-15,
-1.));
#7093=DIRECTION('ref_axis',(-1.33242458232479E-31,1.,-1.25092047100568E-15));
#7094=DIRECTION('center_axis',(0.,0.,-1.));
#7095=DIRECTION('ref_axis',(-1.,0.,0.));
#7096=DIRECTION('center_axis',(0.,0.,-1.));
#7097=DIRECTION('ref_axis',(-1.,0.,0.));
#7098=DIRECTION('center_axis',(2.91605317093441E-16,-1.78680073022012E-15,
-1.));
#7099=DIRECTION('ref_axis',(-4.81742820615958E-33,1.,-1.78680073022012E-15));
#7100=DIRECTION('center_axis',(-4.63562821373958E-16,-1.37740009788611E-15,
-1.));
#7101=DIRECTION('ref_axis',(1.06074921525593E-31,1.,-1.37740009788611E-15));
#7102=DIRECTION('center_axis',(0.,0.,-1.));
#7103=DIRECTION('ref_axis',(-1.,0.,0.));
#7104=DIRECTION('center_axis',(-1.40161216532447E-15,1.14593797759164E-15,
-1.));
#7105=DIRECTION('ref_axis',(-1.,1.10956705583637E-32,1.40161216532447E-15));
#7106=DIRECTION('center_axis',(3.28364901125325E-16,-8.43563346362936E-16,
-1.));
#7107=DIRECTION('ref_axis',(-6.20431423727392E-33,1.,-8.43563346362936E-16));
#7108=DIRECTION('center_axis',(0.,0.,-1.));
#7109=DIRECTION('ref_axis',(-1.,0.,0.));
#7110=DIRECTION('center_axis',(0.,0.,-1.));
#7111=DIRECTION('ref_axis',(-1.,0.,0.));
#7112=DIRECTION('center_axis',(-1.60923747916479E-15,8.29484928207641E-16,
-1.));
#7113=DIRECTION('ref_axis',(-1.,-1.60052481607801E-33,1.60923747916479E-15));
#7114=DIRECTION('center_axis',(9.93152043710262E-16,-1.51371712302742E-15,
-1.));
#7115=DIRECTION('ref_axis',(-1.50815602913865E-32,1.,-1.51371712302742E-15));
#7116=DIRECTION('center_axis',(0.,0.,-1.));
#7117=DIRECTION('ref_axis',(-1.,0.,0.));
#7118=DIRECTION('center_axis',(0.,0.,-1.));
#7119=DIRECTION('ref_axis',(-1.,0.,0.));
#7120=DIRECTION('center_axis',(-8.7326569659373E-16,2.3838970357535E-16,
-1.));
#7121=DIRECTION('ref_axis',(-1.,-2.57646307002641E-33,8.7326569659373E-16));
#7122=DIRECTION('center_axis',(6.43084387593756E-16,-6.37075425716023E-16,
-1.));
#7123=DIRECTION('ref_axis',(-1.,-1.009271785482E-32,-6.43084387593756E-16));
#7124=DIRECTION('center_axis',(0.,0.,-1.));
#7125=DIRECTION('ref_axis',(-1.,0.,0.));
#7126=DIRECTION('center_axis',(0.,0.,-1.));
#7127=DIRECTION('ref_axis',(-1.,0.,0.));
#7128=DIRECTION('center_axis',(7.61486879733257E-16,-4.89449036787473E-16,
-1.));
#7129=DIRECTION('ref_axis',(-1.,-8.14289481143214E-33,-7.61486879733257E-16));
#7130=DIRECTION('center_axis',(0.,0.,-1.));
#7131=DIRECTION('ref_axis',(-1.,0.,0.));
#7132=DIRECTION('center_axis',(0.,0.,-1.));
#7133=DIRECTION('ref_axis',(-1.,0.,0.));
#7134=DIRECTION('center_axis',(1.69321748241794E-15,-6.40862752628506E-16,
-1.));
#7135=DIRECTION('ref_axis',(-1.,-4.80921258844117E-33,-1.69321748241794E-15));
#7136=DIRECTION('center_axis',(0.,0.,-1.));
#7137=DIRECTION('ref_axis',(-1.,0.,0.));
#7138=DIRECTION('center_axis',(0.,0.,-1.));
#7139=DIRECTION('ref_axis',(-1.,0.,0.));
#7140=DIRECTION('center_axis',(0.,0.,-1.));
#7141=DIRECTION('ref_axis',(-1.,0.,0.));
#7142=DIRECTION('center_axis',(-8.4660874120897E-16,-3.20431376314254E-16,
-1.));
#7143=DIRECTION('ref_axis',(-1.,-5.07857362029003E-33,8.4660874120897E-16));
#7144=DIRECTION('center_axis',(1.78945947642876E-15,-2.74818654191543E-16,
-1.));
#7145=DIRECTION('ref_axis',(-1.,3.80943324177873E-33,-1.78945947642876E-15));
#7146=DIRECTION('center_axis',(1.16673654887522E-15,-8.66514480280381E-16,
-1.));
#7147=DIRECTION('ref_axis',(-1.,-8.31157122874193E-32,-1.16673654887522E-15));
#7148=DIRECTION('center_axis',(0.,0.,-1.));
#7149=DIRECTION('ref_axis',(-1.,0.,0.));
#7150=DIRECTION('center_axis',(0.,0.,-1.));
#7151=DIRECTION('ref_axis',(-1.,0.,0.));
#7152=DIRECTION('center_axis',(-7.61486879733269E-16,-4.89449036787465E-16,
-1.));
#7153=DIRECTION('ref_axis',(-1.,8.14289481143968E-33,7.61486879733269E-16));
#7154=DIRECTION('center_axis',(1.80749350454039E-15,1.03236338159813E-16,
-1.));
#7155=DIRECTION('ref_axis',(-1.,4.30743575606662E-34,-1.80749350454039E-15));
#7156=DIRECTION('center_axis',(0.,0.,-1.));
#7157=DIRECTION('ref_axis',(-1.,0.,0.));
#7158=DIRECTION('center_axis',(0.,0.,-1.));
#7159=DIRECTION('ref_axis',(-1.,0.,0.));
#7160=DIRECTION('center_axis',(0.,0.,-1.));
#7161=DIRECTION('ref_axis',(-1.,0.,0.));
#7162=DIRECTION('center_axis',(-6.43084387593765E-16,-6.37075425716018E-16,
-1.));
#7163=DIRECTION('ref_axis',(-1.,1.00927178548269E-32,6.43084387593765E-16));
#7164=DIRECTION('center_axis',(1.74653139318747E-15,4.76779407150673E-16,
-1.));
#7165=DIRECTION('ref_axis',(-1.,-8.38515567292817E-33,-1.74653139318747E-15));
#7166=DIRECTION('center_axis',(0.,0.,-1.));
#7167=DIRECTION('ref_axis',(-1.,0.,0.));
#7168=DIRECTION('center_axis',(0.,0.,-1.));
#7169=DIRECTION('ref_axis',(-1.,0.,0.));
#7170=DIRECTION('center_axis',(1.3675338218833E-16,1.44686558860067E-15,
-1.));
#7171=DIRECTION('ref_axis',(2.17929987622515E-32,1.,1.44686558860067E-15));
#7172=DIRECTION('center_axis',(-9.93152043710302E-16,-1.51371712302744E-15,
-1.));
#7173=DIRECTION('ref_axis',(1.50815602913434E-32,1.,-1.51371712302744E-15));
#7174=DIRECTION('center_axis',(1.60923747916481E-15,8.29484928207625E-16,
-1.));
#7175=DIRECTION('ref_axis',(-1.,1.60052481611945E-33,-1.60923747916481E-15));
#7176=DIRECTION('center_axis',(1.45323412840514E-15,-1.52344036793355E-17,
-1.));
#7177=DIRECTION('ref_axis',(-1.,2.33073141122416E-33,-1.45323412840514E-15));
#7178=DIRECTION('center_axis',(0.,0.,-1.));
#7179=DIRECTION('ref_axis',(-1.,0.,0.));
#7180=DIRECTION('center_axis',(0.,0.,-1.));
#7181=DIRECTION('ref_axis',(-1.,0.,0.));
#7182=DIRECTION('center_axis',(-6.56729802250671E-16,-1.68712669272587E-15,
-1.));
#7183=DIRECTION('ref_axis',(-9.28280238059528E-34,1.,-1.68712669272587E-15));
#7184=DIRECTION('center_axis',(1.4016121653245E-15,1.14593797759163E-15,
-1.));
#7185=DIRECTION('ref_axis',(-1.,-1.1095670558325E-32,-1.4016121653245E-15));
#7186=DIRECTION('center_axis',(0.,0.,-1.));
#7187=DIRECTION('ref_axis',(-1.,0.,0.));
#7188=DIRECTION('center_axis',(0.,0.,-1.));
#7189=DIRECTION('ref_axis',(-1.,0.,0.));
#7190=DIRECTION('center_axis',(0.,0.,-1.));
#7191=DIRECTION('ref_axis',(-1.,0.,0.));
#7192=DIRECTION('center_axis',(0.,0.,-1.));
#7193=DIRECTION('ref_axis',(-1.,0.,0.));
#7194=DIRECTION('center_axis',(5.66364837089046E-16,7.06154019267162E-16,
-1.));
#7195=DIRECTION('ref_axis',(-2.86938317198595E-34,1.,7.06154019267162E-16));
#7196=DIRECTION('center_axis',(0.,0.,-1.));
#7197=DIRECTION('ref_axis',(-1.,0.,0.));
#7198=DIRECTION('center_axis',(0.,0.,-1.));
#7199=DIRECTION('ref_axis',(-1.,0.,0.));
#7200=DIRECTION('center_axis',(0.,0.,-1.));
#7201=DIRECTION('ref_axis',(-1.,0.,0.));
#7202=DIRECTION('center_axis',(4.31318598491376E-17,-9.04191500891285E-16,
-1.));
#7203=DIRECTION('ref_axis',(1.09164579340007E-34,1.,-9.04191500891285E-16));
#7204=DIRECTION('center_axis',(4.07170730415051E-16,8.0847673059362E-16,
-1.));
#7205=DIRECTION('ref_axis',(6.01739504655179E-33,1.,8.0847673059362E-16));
#7206=DIRECTION('center_axis',(0.,0.,-1.));
#7207=DIRECTION('ref_axis',(-1.,0.,0.));
#7208=DIRECTION('center_axis',(0.,0.,-1.));
#7209=DIRECTION('ref_axis',(-1.,0.,0.));
#7210=DIRECTION('center_axis',(0.,0.,-1.));
#7211=DIRECTION('ref_axis',(-1.,0.,0.));
#7212=DIRECTION('center_axis',(2.30181308999977E-16,-8.75465129291365E-16,
-1.));
#7213=DIRECTION('ref_axis',(2.99401685849273E-33,1.,-8.75465129291365E-16));
#7214=DIRECTION('center_axis',(2.30181308999981E-16,8.75465129291358E-16,
-1.));
#7215=DIRECTION('ref_axis',(-2.99401685849028E-33,1.,8.75465129291358E-16));
#7216=DIRECTION('center_axis',(9.83724801784613E-16,1.06976961695994E-15,
-1.));
#7217=DIRECTION('ref_axis',(1.03029779618232E-33,1.,1.06976961695994E-15));
#7218=DIRECTION('center_axis',(0.,0.,-1.));
#7219=DIRECTION('ref_axis',(-1.,0.,0.));
#7220=DIRECTION('center_axis',(1.18464566449553E-15,-8.41864697328891E-16,
-1.));
#7221=DIRECTION('ref_axis',(-1.,-9.58283674537864E-32,-1.18464566449553E-15));
#7222=DIRECTION('center_axis',(4.07170730415049E-16,-8.08476730593625E-16,
-1.));
#7223=DIRECTION('ref_axis',(-6.01739504655004E-33,1.,-8.08476730593625E-16));
#7224=DIRECTION('center_axis',(8.62637196982854E-17,1.80838300178258E-15,
-1.));
#7225=DIRECTION('ref_axis',(-4.36658317360796E-34,1.,1.80838300178258E-15));
#7226=DIRECTION('center_axis',(0.,0.,-1.));
#7227=DIRECTION('ref_axis',(-1.,0.,0.));
#7228=DIRECTION('center_axis',(0.,0.,-1.));
#7229=DIRECTION('ref_axis',(-1.,0.,0.));
#7230=DIRECTION('center_axis',(0.,0.,-1.));
#7231=DIRECTION('ref_axis',(-1.,0.,0.));
#7232=DIRECTION('center_axis',(0.,0.,-1.));
#7233=DIRECTION('ref_axis',(-1.,0.,0.));
#7234=DIRECTION('center_axis',(-2.91605317093461E-16,1.78680073022012E-15,
-1.));
#7235=DIRECTION('ref_axis',(-4.81742820615809E-33,1.,1.78680073022012E-15));
#7236=DIRECTION('center_axis',(4.63562821373925E-16,1.3774000978861E-15,
-1.));
#7237=DIRECTION('ref_axis',(1.06074921525595E-31,1.,1.3774000978861E-15));
#7238=DIRECTION('center_axis',(0.,0.,-1.));
#7239=DIRECTION('ref_axis',(-1.,0.,0.));
#7240=DIRECTION('center_axis',(0.,0.,-1.));
#7241=DIRECTION('ref_axis',(-1.,0.,0.));
#7242=DIRECTION('center_axis',(7.00806082662239E-16,-5.72968988795806E-16,
-1.));
#7243=DIRECTION('ref_axis',(-1.,2.77391763959504E-33,-7.00806082662239E-16));
#7244=DIRECTION('center_axis',(0.,0.,-1.));
#7245=DIRECTION('ref_axis',(-1.,0.,0.));
#7246=DIRECTION('center_axis',(0.,0.,-1.));
#7247=DIRECTION('ref_axis',(-1.,0.,0.));
#7248=DIRECTION('center_axis',(0.,0.,-1.));
#7249=DIRECTION('ref_axis',(-1.,0.,0.));
#7250=DIRECTION('center_axis',(0.,0.,-1.));
#7251=DIRECTION('ref_axis',(-1.,0.,0.));
#7252=DIRECTION('',(1.13134139737618E-16,-1.,0.));
#7253=DIRECTION('',(-1.,0.,0.));
#7254=DIRECTION('',(1.13134139737618E-16,1.,0.));
#7255=DIRECTION('center_axis',(0.,0.,-1.));
#7256=DIRECTION('ref_axis',(-1.,0.,0.));
#7257=DIRECTION('',(0.,0.,-1.));
#7258=DIRECTION('center_axis',(0.,0.,1.));
#7259=DIRECTION('ref_axis',(1.,0.,0.));
#7260=DIRECTION('',(0.,0.,1.));
#7261=DIRECTION('center_axis',(0.,0.,1.));
#7262=DIRECTION('ref_axis',(1.,0.,0.));
#7263=DIRECTION('',(0.,0.,-1.));
#7264=DIRECTION('center_axis',(0.,0.,1.));
#7265=DIRECTION('ref_axis',(1.,0.,0.));
#7266=DIRECTION('',(0.,0.,-1.));
#7267=DIRECTION('',(0.,0.,1.));
#7268=DIRECTION('center_axis',(0.,0.,-1.));
#7269=DIRECTION('ref_axis',(-1.,0.,0.));
#7270=DIRECTION('center_axis',(0.,0.,-1.));
#7271=DIRECTION('ref_axis',(-1.,0.,0.));
#7272=DIRECTION('center_axis',(0.,0.,1.));
#7273=DIRECTION('ref_axis',(-0.988411742041742,-0.151796667269113,0.));
#7274=DIRECTION('',(0.,0.,-1.));
#7275=DIRECTION('center_axis',(0.,0.,1.));
#7276=DIRECTION('ref_axis',(1.,0.,0.));
#7277=DIRECTION('',(0.,0.,1.));
#7278=DIRECTION('center_axis',(0.,0.,-1.));
#7279=DIRECTION('ref_axis',(-1.,0.,0.));
#7280=DIRECTION('',(0.,0.,-1.));
#7281=DIRECTION('center_axis',(0.,0.,1.));
#7282=DIRECTION('ref_axis',(1.,0.,0.));
#7283=DIRECTION('',(0.,0.,1.));
#7284=DIRECTION('center_axis',(0.,0.,-1.));
#7285=DIRECTION('ref_axis',(0.802811069346193,0.596233500346318,0.));
#7286=DIRECTION('center_axis',(0.,0.,1.));
#7287=DIRECTION('ref_axis',(1.,0.,0.));
#7288=DIRECTION('center_axis',(0.,0.,1.));
#7289=DIRECTION('ref_axis',(1.,0.,0.));
#7290=DIRECTION('',(0.,0.,1.));
#7291=DIRECTION('center_axis',(0.,0.,-1.));
#7292=DIRECTION('ref_axis',(-1.,0.,0.));
#7293=DIRECTION('',(0.,0.,-1.));
#7294=DIRECTION('center_axis',(0.,0.,1.));
#7295=DIRECTION('ref_axis',(1.,0.,0.));
#7296=DIRECTION('center_axis',(0.,0.,1.));
#7297=DIRECTION('ref_axis',(1.,0.,0.));
#7298=DIRECTION('center_axis',(0.,0.,1.));
#7299=DIRECTION('ref_axis',(1.,0.,0.));
#7300=DIRECTION('',(0.,0.,1.));
#7301=DIRECTION('center_axis',(0.,0.,-1.));
#7302=DIRECTION('ref_axis',(-1.,0.,0.));
#7303=DIRECTION('',(0.,0.,-1.));
#7304=DIRECTION('center_axis',(0.,0.,1.));
#7305=DIRECTION('ref_axis',(1.,0.,0.));
#7306=DIRECTION('center_axis',(0.,0.,1.));
#7307=DIRECTION('ref_axis',(1.,0.,0.));
#7308=DIRECTION('center_axis',(0.,0.,1.));
#7309=DIRECTION('ref_axis',(1.,0.,0.));
#7310=DIRECTION('',(0.,0.,1.));
#7311=DIRECTION('center_axis',(0.,0.,-1.));
#7312=DIRECTION('ref_axis',(-1.,0.,0.));
#7313=DIRECTION('',(0.,0.,-1.));
#7314=DIRECTION('center_axis',(0.,0.,1.));
#7315=DIRECTION('ref_axis',(1.,0.,0.));
#7316=DIRECTION('center_axis',(0.,0.,1.));
#7317=DIRECTION('ref_axis',(1.,0.,0.));
#7318=DIRECTION('center_axis',(0.,0.,1.));
#7319=DIRECTION('ref_axis',(1.,0.,0.));
#7320=DIRECTION('',(0.,0.,1.));
#7321=DIRECTION('center_axis',(0.,0.,-1.));
#7322=DIRECTION('ref_axis',(-1.,0.,0.));
#7323=DIRECTION('',(0.,0.,-1.));
#7324=DIRECTION('center_axis',(0.,0.,1.));
#7325=DIRECTION('ref_axis',(1.,0.,0.));
#7326=DIRECTION('center_axis',(0.,0.,1.));
#7327=DIRECTION('ref_axis',(1.,0.,0.));
#7328=DIRECTION('center_axis',(0.,0.,1.));
#7329=DIRECTION('ref_axis',(1.,0.,0.));
#7330=DIRECTION('',(0.,0.,1.));
#7331=DIRECTION('center_axis',(0.,0.,-1.));
#7332=DIRECTION('ref_axis',(-1.,0.,0.));
#7333=DIRECTION('',(0.,0.,-1.));
#7334=DIRECTION('center_axis',(0.,0.,1.));
#7335=DIRECTION('ref_axis',(1.,0.,0.));
#7336=DIRECTION('center_axis',(0.,0.,1.));
#7337=DIRECTION('ref_axis',(1.,0.,0.));
#7338=DIRECTION('',(0.,0.,-1.));
#7339=DIRECTION('center_axis',(0.,0.,1.));
#7340=DIRECTION('ref_axis',(1.,0.,0.));
#7341=DIRECTION('center_axis',(0.,0.,1.));
#7342=DIRECTION('ref_axis',(1.,0.,0.));
#7343=DIRECTION('',(0.,0.,1.));
#7344=DIRECTION('center_axis',(0.,0.,-1.));
#7345=DIRECTION('ref_axis',(-1.,0.,0.));
#7346=DIRECTION('center_axis',(0.,0.,1.));
#7347=DIRECTION('ref_axis',(1.,0.,0.));
#7348=DIRECTION('',(0.,0.,-1.));
#7349=DIRECTION('center_axis',(0.,0.,1.));
#7350=DIRECTION('ref_axis',(1.,0.,0.));
#7351=DIRECTION('center_axis',(0.,0.,1.));
#7352=DIRECTION('ref_axis',(1.,0.,0.));
#7353=DIRECTION('',(0.,0.,1.));
#7354=DIRECTION('center_axis',(0.,0.,-1.));
#7355=DIRECTION('ref_axis',(-1.,0.,0.));
#7356=DIRECTION('center_axis',(0.,0.,1.));
#7357=DIRECTION('ref_axis',(1.,0.,0.));
#7358=DIRECTION('',(0.,0.,-1.));
#7359=DIRECTION('center_axis',(0.,0.,1.));
#7360=DIRECTION('ref_axis',(1.,0.,0.));
#7361=DIRECTION('center_axis',(0.,0.,1.));
#7362=DIRECTION('ref_axis',(1.,0.,0.));
#7363=DIRECTION('',(0.,0.,1.));
#7364=DIRECTION('center_axis',(0.,0.,-1.));
#7365=DIRECTION('ref_axis',(-1.,0.,0.));
#7366=DIRECTION('center_axis',(0.,0.,1.));
#7367=DIRECTION('ref_axis',(1.,0.,0.));
#7368=DIRECTION('',(0.,0.,-1.));
#7369=DIRECTION('center_axis',(0.,0.,1.));
#7370=DIRECTION('ref_axis',(1.,0.,0.));
#7371=DIRECTION('center_axis',(0.,0.,1.));
#7372=DIRECTION('ref_axis',(1.,0.,0.));
#7373=DIRECTION('',(0.,0.,1.));
#7374=DIRECTION('center_axis',(0.,0.,-1.));
#7375=DIRECTION('ref_axis',(-1.,0.,0.));
#7376=DIRECTION('center_axis',(0.,0.,1.));
#7377=DIRECTION('ref_axis',(1.,0.,0.));
#7378=DIRECTION('',(0.,0.,-1.));
#7379=DIRECTION('center_axis',(0.,0.,1.));
#7380=DIRECTION('ref_axis',(1.,0.,0.));
#7381=DIRECTION('center_axis',(0.,0.,1.));
#7382=DIRECTION('ref_axis',(1.,0.,0.));
#7383=DIRECTION('',(0.,0.,1.));
#7384=DIRECTION('center_axis',(0.,0.,-1.));
#7385=DIRECTION('ref_axis',(-1.,0.,0.));
#7386=DIRECTION('center_axis',(0.,0.,1.));
#7387=DIRECTION('ref_axis',(1.,0.,0.));
#7388=DIRECTION('',(0.,0.,-1.));
#7389=DIRECTION('center_axis',(0.,0.,1.));
#7390=DIRECTION('ref_axis',(1.,0.,0.));
#7391=DIRECTION('',(0.,0.,1.));
#7392=DIRECTION('center_axis',(0.,0.,-1.));
#7393=DIRECTION('ref_axis',(-1.,0.,0.));
#7394=DIRECTION('center_axis',(0.,0.,1.));
#7395=DIRECTION('ref_axis',(1.,0.,0.));
#7396=DIRECTION('',(0.,0.,-1.));
#7397=DIRECTION('center_axis',(0.,0.,1.));
#7398=DIRECTION('ref_axis',(1.,0.,0.));
#7399=DIRECTION('',(0.,0.,1.));
#7400=DIRECTION('center_axis',(0.,0.,-1.));
#7401=DIRECTION('ref_axis',(-1.,0.,0.));
#7402=DIRECTION('center_axis',(0.,0.,1.));
#7403=DIRECTION('ref_axis',(1.,0.,0.));
#7404=DIRECTION('',(0.,0.,1.));
#7405=DIRECTION('center_axis',(0.,0.,-1.));
#7406=DIRECTION('ref_axis',(-1.,0.,0.));
#7407=DIRECTION('',(0.,0.,-1.));
#7408=DIRECTION('center_axis',(0.,0.,1.));
#7409=DIRECTION('ref_axis',(1.,0.,0.));
#7410=DIRECTION('center_axis',(0.,0.,1.));
#7411=DIRECTION('ref_axis',(1.,0.,0.));
#7412=DIRECTION('',(0.,0.,1.));
#7413=DIRECTION('center_axis',(0.,0.,-1.));
#7414=DIRECTION('ref_axis',(-1.,0.,0.));
#7415=DIRECTION('',(0.,0.,-1.));
#7416=DIRECTION('center_axis',(0.,0.,1.));
#7417=DIRECTION('ref_axis',(1.,0.,0.));
#7418=DIRECTION('center_axis',(0.,0.,1.));
#7419=DIRECTION('ref_axis',(1.,0.,0.));
#7420=DIRECTION('',(0.,0.,-1.));
#7421=DIRECTION('center_axis',(0.,0.,1.));
#7422=DIRECTION('ref_axis',(1.,0.,0.));
#7423=DIRECTION('',(0.,0.,1.));
#7424=DIRECTION('center_axis',(0.,0.,-1.));
#7425=DIRECTION('ref_axis',(-1.,0.,0.));
#7426=DIRECTION('',(0.,0.,-1.));
#7427=DIRECTION('center_axis',(0.,0.,1.));
#7428=DIRECTION('ref_axis',(1.,0.,0.));
#7429=DIRECTION('',(0.,0.,1.));
#7430=DIRECTION('center_axis',(0.,0.,-1.));
#7431=DIRECTION('ref_axis',(-1.,0.,0.));
#7432=DIRECTION('center_axis',(0.,0.,1.));
#7433=DIRECTION('ref_axis',(1.,0.,0.));
#7434=DIRECTION('',(0.,0.,-1.));
#7435=DIRECTION('center_axis',(0.,0.,1.));
#7436=DIRECTION('ref_axis',(-0.98841174204174,0.151796667269121,0.));
#7437=DIRECTION('',(0.,0.,1.));
#7438=DIRECTION('center_axis',(0.,0.,-1.));
#7439=DIRECTION('ref_axis',(0.802811069346192,-0.596233500346319,0.));
#7440=DIRECTION('',(0.,0.,-1.));
#7441=DIRECTION('center_axis',(0.,0.,1.));
#7442=DIRECTION('ref_axis',(1.,0.,0.));
#7443=DIRECTION('',(0.,0.,1.));
#7444=DIRECTION('center_axis',(0.,0.,-1.));
#7445=DIRECTION('ref_axis',(-1.,0.,0.));
#7446=DIRECTION('center_axis',(0.,0.,1.));
#7447=DIRECTION('ref_axis',(1.,0.,0.));
#7448=DIRECTION('',(0.,0.,-1.));
#7449=DIRECTION('center_axis',(0.,0.,1.));
#7450=DIRECTION('ref_axis',(1.,0.,0.));
#7451=DIRECTION('',(0.,0.,1.));
#7452=DIRECTION('center_axis',(0.,0.,-1.));
#7453=DIRECTION('ref_axis',(0.999945056799679,-0.0104825274569905,0.));
#7454=DIRECTION('',(0.,0.,-1.));
#7455=DIRECTION('center_axis',(0.,0.,1.));
#7456=DIRECTION('ref_axis',(1.,0.,0.));
#7457=DIRECTION('',(0.,0.,1.));
#7458=DIRECTION('center_axis',(0.,0.,-1.));
#7459=DIRECTION('ref_axis',(-1.,0.,0.));
#7460=DIRECTION('center_axis',(0.,0.,1.));
#7461=DIRECTION('ref_axis',(1.,0.,0.));
#7462=DIRECTION('',(0.,0.,-1.));
#7463=DIRECTION('center_axis',(0.,0.,1.));
#7464=DIRECTION('ref_axis',(1.,0.,0.));
#7465=DIRECTION('',(0.,0.,1.));
#7466=DIRECTION('center_axis',(0.,0.,-1.));
#7467=DIRECTION('ref_axis',(0.980273298181862,0.1976468084024,0.));
#7468=DIRECTION('',(0.,0.,-1.));
#7469=DIRECTION('center_axis',(0.,0.,1.));
#7470=DIRECTION('ref_axis',(1.,0.,0.));
#7471=DIRECTION('',(0.,0.,1.));
#7472=DIRECTION('center_axis',(0.,0.,-1.));
#7473=DIRECTION('ref_axis',(-1.,0.,0.));
#7474=DIRECTION('center_axis',(0.,0.,1.));
#7475=DIRECTION('ref_axis',(1.,0.,0.));
#7476=DIRECTION('',(0.,0.,-1.));
#7477=DIRECTION('center_axis',(0.,0.,1.));
#7478=DIRECTION('ref_axis',(1.,0.,0.));
#7479=DIRECTION('',(0.,0.,1.));
#7480=DIRECTION('center_axis',(0.,0.,-1.));
#7481=DIRECTION('ref_axis',(0.975914418166608,-0.218153726565768,0.));
#7482=DIRECTION('',(0.,0.,-1.));
#7483=DIRECTION('center_axis',(0.,0.,1.));
#7484=DIRECTION('ref_axis',(1.,0.,0.));
#7485=DIRECTION('',(0.,0.,1.));
#7486=DIRECTION('center_axis',(0.,0.,-1.));
#7487=DIRECTION('ref_axis',(-1.,0.,0.));
#7488=DIRECTION('center_axis',(0.,0.,1.));
#7489=DIRECTION('ref_axis',(1.,0.,0.));
#7490=DIRECTION('',(0.,0.,-1.));
#7491=DIRECTION('center_axis',(0.,0.,1.));
#7492=DIRECTION('ref_axis',(-0.998372875767673,-0.0570228106233482,0.));
#7493=DIRECTION('',(0.,0.,1.));
#7494=DIRECTION('center_axis',(0.,0.,-1.));
#7495=DIRECTION('ref_axis',(0.909231636502713,-0.416290561005889,0.));
#7496=DIRECTION('',(0.,0.,-1.));
#7497=DIRECTION('center_axis',(0.,0.,1.));
#7498=DIRECTION('ref_axis',(1.,0.,0.));
#7499=DIRECTION('',(0.,0.,1.));
#7500=DIRECTION('center_axis',(0.,0.,-1.));
#7501=DIRECTION('ref_axis',(-1.,0.,0.));
#7502=DIRECTION('center_axis',(0.,0.,1.));
#7503=DIRECTION('ref_axis',(1.,0.,0.));
#7504=DIRECTION('',(0.,0.,-1.));
#7505=DIRECTION('center_axis',(0.,0.,1.));
#7506=DIRECTION('ref_axis',(1.,0.,0.));
#7507=DIRECTION('',(0.,0.,1.));
#7508=DIRECTION('center_axis',(0.,0.,-1.));
#7509=DIRECTION('ref_axis',(0.917758892560327,0.397138030319992,0.));
#7510=DIRECTION('',(0.,0.,-1.));
#7511=DIRECTION('center_axis',(0.,0.,1.));
#7512=DIRECTION('ref_axis',(1.,0.,0.));
#7513=DIRECTION('',(0.,0.,1.));
#7514=DIRECTION('center_axis',(0.,0.,-1.));
#7515=DIRECTION('ref_axis',(-1.,0.,0.));
#7516=DIRECTION('center_axis',(0.,0.,1.));
#7517=DIRECTION('ref_axis',(1.,0.,0.));
#7518=DIRECTION('',(0.,0.,-1.));
#7519=DIRECTION('center_axis',(0.,0.,1.));
#7520=DIRECTION('ref_axis',(1.,0.,0.));
#7521=DIRECTION('',(0.,0.,1.));
#7522=DIRECTION('center_axis',(0.,0.,-1.));
#7523=DIRECTION('ref_axis',(0.815134019438133,0.579272414632902,0.));
#7524=DIRECTION('',(0.,0.,-1.));
#7525=DIRECTION('center_axis',(0.,0.,1.));
#7526=DIRECTION('ref_axis',(1.,0.,0.));
#7527=DIRECTION('',(0.,0.,1.));
#7528=DIRECTION('center_axis',(0.,0.,-1.));
#7529=DIRECTION('ref_axis',(-1.,0.,0.));
#7530=DIRECTION('center_axis',(0.,0.,1.));
#7531=DIRECTION('ref_axis',(1.,0.,0.));
#7532=DIRECTION('',(0.,0.,-1.));
#7533=DIRECTION('center_axis',(0.,0.,1.));
#7534=DIRECTION('ref_axis',(1.,0.,0.));
#7535=DIRECTION('',(0.,0.,1.));
#7536=DIRECTION('center_axis',(0.,0.,-1.));
#7537=DIRECTION('ref_axis',(-1.,0.,0.));
#7538=DIRECTION('',(0.,0.,-1.));
#7539=DIRECTION('center_axis',(0.,0.,1.));
#7540=DIRECTION('ref_axis',(1.,0.,0.));
#7541=DIRECTION('',(0.,0.,1.));
#7542=DIRECTION('center_axis',(0.,0.,-1.));
#7543=DIRECTION('ref_axis',(0.815134019438124,-0.579272414632915,0.));
#7544=DIRECTION('center_axis',(0.,0.,1.));
#7545=DIRECTION('ref_axis',(1.,0.,0.));
#7546=DIRECTION('',(0.,0.,-1.));
#7547=DIRECTION('center_axis',(0.,0.,1.));
#7548=DIRECTION('ref_axis',(1.,0.,0.));
#7549=DIRECTION('',(0.,0.,1.));
#7550=DIRECTION('center_axis',(0.,0.,-1.));
#7551=DIRECTION('ref_axis',(-1.,0.,0.));
#7552=DIRECTION('',(0.,0.,-1.));
#7553=DIRECTION('center_axis',(0.,0.,1.));
#7554=DIRECTION('ref_axis',(1.,0.,0.));
#7555=DIRECTION('',(0.,0.,1.));
#7556=DIRECTION('center_axis',(0.,0.,-1.));
#7557=DIRECTION('ref_axis',(0.917758892560322,-0.397138030320002,0.));
#7558=DIRECTION('center_axis',(0.,0.,1.));
#7559=DIRECTION('ref_axis',(-0.998372875767673,0.0570228106233547,0.));
#7560=DIRECTION('',(0.,0.,-1.));
#7561=DIRECTION('center_axis',(0.,0.,1.));
#7562=DIRECTION('ref_axis',(1.,0.,0.));
#7563=DIRECTION('',(0.,0.,1.));
#7564=DIRECTION('center_axis',(0.,0.,-1.));
#7565=DIRECTION('ref_axis',(-1.,0.,0.));
#7566=DIRECTION('',(0.,0.,-1.));
#7567=DIRECTION('center_axis',(0.,0.,1.));
#7568=DIRECTION('ref_axis',(1.,0.,0.));
#7569=DIRECTION('',(0.,0.,1.));
#7570=DIRECTION('center_axis',(0.,0.,-1.));
#7571=DIRECTION('ref_axis',(0.909231636502717,0.416290561005881,0.));
#7572=DIRECTION('center_axis',(0.,0.,1.));
#7573=DIRECTION('ref_axis',(1.,0.,0.));
#7574=DIRECTION('',(0.,0.,-1.));
#7575=DIRECTION('center_axis',(0.,0.,1.));
#7576=DIRECTION('ref_axis',(1.,0.,0.));
#7577=DIRECTION('',(0.,0.,1.));
#7578=DIRECTION('center_axis',(0.,0.,-1.));
#7579=DIRECTION('ref_axis',(-1.,0.,0.));
#7580=DIRECTION('',(0.,0.,-1.));
#7581=DIRECTION('center_axis',(0.,0.,1.));
#7582=DIRECTION('ref_axis',(1.,0.,0.));
#7583=DIRECTION('',(0.,0.,1.));
#7584=DIRECTION('center_axis',(0.,0.,-1.));
#7585=DIRECTION('ref_axis',(0.975914418166611,0.218153726565752,0.));
#7586=DIRECTION('center_axis',(0.,0.,1.));
#7587=DIRECTION('ref_axis',(1.,0.,0.));
#7588=DIRECTION('',(0.,0.,-1.));
#7589=DIRECTION('center_axis',(0.,0.,1.));
#7590=DIRECTION('ref_axis',(1.,0.,0.));
#7591=DIRECTION('',(0.,0.,1.));
#7592=DIRECTION('center_axis',(0.,0.,-1.));
#7593=DIRECTION('ref_axis',(-1.,0.,0.));
#7594=DIRECTION('',(0.,0.,-1.));
#7595=DIRECTION('center_axis',(0.,0.,1.));
#7596=DIRECTION('ref_axis',(1.,0.,0.));
#7597=DIRECTION('',(0.,0.,1.));
#7598=DIRECTION('center_axis',(0.,0.,-1.));
#7599=DIRECTION('ref_axis',(0.98027329818186,-0.19764680840241,0.));
#7600=DIRECTION('center_axis',(0.,0.,1.));
#7601=DIRECTION('ref_axis',(1.,0.,0.));
#7602=DIRECTION('',(0.,0.,-1.));
#7603=DIRECTION('center_axis',(0.,0.,1.));
#7604=DIRECTION('ref_axis',(1.,0.,0.));
#7605=DIRECTION('',(0.,0.,1.));
#7606=DIRECTION('center_axis',(0.,0.,-1.));
#7607=DIRECTION('ref_axis',(-1.,0.,0.));
#7608=DIRECTION('',(0.,0.,-1.));
#7609=DIRECTION('center_axis',(0.,0.,1.));
#7610=DIRECTION('ref_axis',(1.,0.,0.));
#7611=DIRECTION('',(0.,0.,1.));
#7612=DIRECTION('center_axis',(0.,0.,-1.));
#7613=DIRECTION('ref_axis',(0.999945056799679,0.010482527456989,0.));
#7614=DIRECTION('center_axis',(0.,1.,0.));
#7615=DIRECTION('ref_axis',(0.,0.,1.));
#7616=DIRECTION('',(0.,0.,1.));
#7617=DIRECTION('',(0.,0.,1.));
#7618=DIRECTION('center_axis',(-1.,-1.13134139737618E-16,0.));
#7619=DIRECTION('ref_axis',(1.13134139737618E-16,-1.,0.));
#7620=DIRECTION('center_axis',(1.,-1.13134139737618E-16,0.));
#7621=DIRECTION('ref_axis',(1.13134139737618E-16,1.,0.));
#7622=DIRECTION('axis',(0.,0.,1.));
#7623=DIRECTION('refdir',(1.,0.,0.));
#7624=DIRECTION('center_axis',(-1.,0.,0.));
#7625=DIRECTION('ref_axis',(0.,0.,1.));
#7626=DIRECTION('center_axis',(-1.,0.,0.));
#7627=DIRECTION('ref_axis',(0.,0.,1.));
#7628=DIRECTION('',(-1.,0.,0.));
#7629=DIRECTION('center_axis',(-1.,0.,0.));
#7630=DIRECTION('ref_axis',(0.,0.,1.));
#7631=DIRECTION('center_axis',(-1.,0.,0.));
#7632=DIRECTION('ref_axis',(0.,0.,1.));
#7633=DIRECTION('center_axis',(-1.,0.,0.));
#7634=DIRECTION('ref_axis',(0.,2.66453525910037E-15,-1.));
#7635=DIRECTION('center_axis',(1.,0.,0.));
#7636=DIRECTION('ref_axis',(0.,0.,1.));
#7637=DIRECTION('center_axis',(1.,0.,0.));
#7638=DIRECTION('ref_axis',(0.,0.,-1.));
#7639=DIRECTION('center_axis',(0.,-0.5,-0.866025403784439));
#7640=DIRECTION('ref_axis',(0.,0.866025403784439,-0.5));
#7641=DIRECTION('',(-1.,0.,0.));
#7642=DIRECTION('',(-1.,0.,0.));
#7643=DIRECTION('center_axis',(0.,0.5,-0.866025403784439));
#7644=DIRECTION('ref_axis',(0.,0.866025403784439,0.5));
#7645=DIRECTION('',(-1.,0.,0.));
#7646=DIRECTION('center_axis',(0.,1.,-4.6225064576528E-16));
#7647=DIRECTION('ref_axis',(0.,4.6225064576528E-16,1.));
#7648=DIRECTION('',(-1.,0.,0.));
#7649=DIRECTION('center_axis',(0.,0.5,0.866025403784439));
#7650=DIRECTION('ref_axis',(0.,-0.866025403784439,0.5));
#7651=DIRECTION('',(-1.,0.,0.));
#7652=DIRECTION('center_axis',(0.,-0.5,0.866025403784439));
#7653=DIRECTION('ref_axis',(0.,-0.866025403784439,-0.5));
#7654=DIRECTION('',(-1.,0.,0.));
#7655=DIRECTION('center_axis',(0.,-1.,3.4668798432396E-16));
#7656=DIRECTION('ref_axis',(0.,-3.4668798432396E-16,-1.));
#7657=DIRECTION('center_axis',(1.,0.,0.));
#7658=DIRECTION('ref_axis',(0.,-1.22464679914735E-16,-1.));
#7659=DIRECTION('center_axis',(1.,0.,0.));
#7660=DIRECTION('ref_axis',(0.,0.,-1.));
#7661=DIRECTION('center_axis',(1.,0.,0.));
#7662=DIRECTION('ref_axis',(0.,0.,1.));
#7663=DIRECTION('center_axis',(1.,0.,0.));
#7664=DIRECTION('ref_axis',(0.,0.,-1.));
#7665=DIRECTION('center_axis',(1.,0.,0.));
#7666=DIRECTION('ref_axis',(0.,0.,1.));
#7667=DIRECTION('center_axis',(1.,0.,0.));
#7668=DIRECTION('ref_axis',(0.,0.,-1.));
#7669=DIRECTION('center_axis',(1.,0.,0.));
#7670=DIRECTION('ref_axis',(0.,0.,1.));
#7671=DIRECTION('center_axis',(-1.,0.,0.));
#7672=DIRECTION('ref_axis',(0.,0.,1.));
#7673=DIRECTION('center_axis',(1.,0.,0.));
#7674=DIRECTION('ref_axis',(0.,0.,1.));
#7675=DIRECTION('center_axis',(1.,0.,0.));
#7676=DIRECTION('ref_axis',(0.,0.,-1.));
#7677=DIRECTION('center_axis',(1.,0.,0.));
#7678=DIRECTION('ref_axis',(0.,0.,-1.));
#7679=DIRECTION('center_axis',(-1.,0.,0.));
#7680=DIRECTION('ref_axis',(0.,1.89882151931499E-15,-1.));
#7681=DIRECTION('center_axis',(-1.,0.,0.));
#7682=DIRECTION('ref_axis',(0.,0.,-1.));
#7683=DIRECTION('center_axis',(-1.,0.,0.));
#7684=DIRECTION('ref_axis',(0.,0.,1.));
#7685=DIRECTION('center_axis',(-1.,0.,0.));
#7686=DIRECTION('ref_axis',(0.,0.,-1.));
#7687=DIRECTION('center_axis',(-1.,0.,0.));
#7688=DIRECTION('ref_axis',(0.,0.,1.));
#7689=DIRECTION('center_axis',(-1.,0.,0.));
#7690=DIRECTION('ref_axis',(0.,0.,1.));
#7691=DIRECTION('center_axis',(-1.,0.,0.));
#7692=DIRECTION('ref_axis',(0.,0.,1.));
#7693=DIRECTION('center_axis',(-1.,0.,0.));
#7694=DIRECTION('ref_axis',(0.,0.,-1.));
#7695=DIRECTION('center_axis',(-1.,0.,0.));
#7696=DIRECTION('ref_axis',(0.,0.,1.));
#7697=DIRECTION('center_axis',(-1.,0.,0.));
#7698=DIRECTION('ref_axis',(0.,0.,-1.));
#7699=DIRECTION('center_axis',(1.,0.,0.));
#7700=DIRECTION('ref_axis',(0.,0.,-1.));
#7701=DIRECTION('axis',(0.,0.,1.));
#7702=DIRECTION('refdir',(1.,0.,0.));
#7703=DIRECTION('center_axis',(0.,0.,-1.));
#7704=DIRECTION('ref_axis',(-1.,0.,0.));
#7705=DIRECTION('center_axis',(0.,0.,1.));
#7706=DIRECTION('ref_axis',(1.,0.,0.));
#7707=DIRECTION('',(0.,0.,-1.));
#7708=DIRECTION('center_axis',(0.,0.,1.));
#7709=DIRECTION('ref_axis',(1.,0.,0.));
#7710=DIRECTION('center_axis',(0.,0.,-1.));
#7711=DIRECTION('ref_axis',(-1.,0.,0.));
#7712=DIRECTION('center_axis',(0.,0.,1.));
#7713=DIRECTION('ref_axis',(1.,0.,0.));
#7714=DIRECTION('',(0.,0.,1.));
#7715=DIRECTION('center_axis',(0.,0.,1.));
#7716=DIRECTION('ref_axis',(1.,0.,0.));
#7717=DIRECTION('center_axis',(0.,0.,-1.));
#7718=DIRECTION('ref_axis',(-1.,0.,0.));
#7719=DIRECTION('center_axis',(0.,0.,1.));
#7720=DIRECTION('ref_axis',(1.,0.,0.));
#7721=DIRECTION('',(0.,0.,-1.));
#7722=DIRECTION('center_axis',(0.,0.,1.));
#7723=DIRECTION('ref_axis',(1.,0.,0.));
#7724=DIRECTION('center_axis',(0.,0.,-1.));
#7725=DIRECTION('ref_axis',(-1.,0.,0.));
#7726=DIRECTION('center_axis',(0.,0.,1.));
#7727=DIRECTION('ref_axis',(1.,0.,0.));
#7728=DIRECTION('',(0.,0.,-1.));
#7729=DIRECTION('center_axis',(0.,0.,1.));
#7730=DIRECTION('ref_axis',(1.,0.,0.));
#7731=DIRECTION('center_axis',(0.,0.,-1.));
#7732=DIRECTION('ref_axis',(-1.,0.,0.));
#7733=DIRECTION('center_axis',(0.,0.,1.));
#7734=DIRECTION('ref_axis',(1.,0.,0.));
#7735=DIRECTION('',(0.,0.,-1.));
#7736=DIRECTION('center_axis',(0.,0.,1.));
#7737=DIRECTION('ref_axis',(1.,0.,0.));
#7738=DIRECTION('center_axis',(0.,0.,-1.));
#7739=DIRECTION('ref_axis',(-1.,0.,0.));
#7740=DIRECTION('center_axis',(0.,0.,1.));
#7741=DIRECTION('ref_axis',(1.,0.,0.));
#7742=DIRECTION('',(0.,0.,-1.));
#7743=DIRECTION('center_axis',(0.,0.,1.));
#7744=DIRECTION('ref_axis',(1.,0.,0.));
#7745=DIRECTION('center_axis',(0.,0.,-1.));
#7746=DIRECTION('ref_axis',(-1.,0.,0.));
#7747=DIRECTION('center_axis',(0.,0.,1.));
#7748=DIRECTION('ref_axis',(1.,0.,0.));
#7749=DIRECTION('',(0.,0.,-1.));
#7750=DIRECTION('center_axis',(0.,0.,1.));
#7751=DIRECTION('ref_axis',(1.,0.,0.));
#7752=DIRECTION('center_axis',(0.,0.,1.));
#7753=DIRECTION('ref_axis',(1.,0.,0.));
#7754=DIRECTION('center_axis',(0.,0.,1.));
#7755=DIRECTION('ref_axis',(1.,0.,0.));
#7756=DIRECTION('center_axis',(0.,0.,1.));
#7757=DIRECTION('ref_axis',(1.,0.,0.));
#7758=DIRECTION('axis',(0.,0.,1.));
#7759=DIRECTION('refdir',(1.,0.,0.));
#7760=DIRECTION('center_axis',(0.,0.,-1.));
#7761=DIRECTION('ref_axis',(-1.,0.,0.));
#7762=DIRECTION('center_axis',(0.,0.,1.));
#7763=DIRECTION('ref_axis',(1.,0.,0.));
#7764=DIRECTION('',(0.,0.,-1.));
#7765=DIRECTION('center_axis',(0.,0.,1.));
#7766=DIRECTION('ref_axis',(1.,0.,0.));
#7767=DIRECTION('center_axis',(0.,0.,-1.));
#7768=DIRECTION('ref_axis',(-1.,0.,0.));
#7769=DIRECTION('center_axis',(0.,0.,1.));
#7770=DIRECTION('ref_axis',(1.,0.,0.));
#7771=DIRECTION('',(0.,0.,1.));
#7772=DIRECTION('center_axis',(0.,0.,1.));
#7773=DIRECTION('ref_axis',(1.,0.,0.));
#7774=DIRECTION('center_axis',(0.,0.,1.));
#7775=DIRECTION('ref_axis',(1.,0.,0.));
#7776=DIRECTION('center_axis',(0.,0.,1.));
#7777=DIRECTION('ref_axis',(1.,0.,0.));
#7778=DIRECTION('axis',(0.,0.,1.));
#7779=DIRECTION('refdir',(1.,0.,0.));
#7780=DIRECTION('center_axis',(0.,0.,-1.));
#7781=DIRECTION('ref_axis',(-1.,0.,0.));
#7782=DIRECTION('center_axis',(0.,0.,1.));
#7783=DIRECTION('ref_axis',(1.,0.,0.));
#7784=DIRECTION('',(0.,0.,1.));
#7785=DIRECTION('center_axis',(0.,0.,1.));
#7786=DIRECTION('ref_axis',(1.,0.,0.));
#7787=DIRECTION('center_axis',(0.,0.,1.));
#7788=DIRECTION('ref_axis',(1.,0.,0.));
#7789=DIRECTION('',(0.500000000000001,0.866025403784438,0.));
#7790=DIRECTION('',(-0.500000000000001,0.866025403784438,0.));
#7791=DIRECTION('',(-1.,0.,0.));
#7792=DIRECTION('',(-0.500000000000001,-0.866025403784438,0.));
#7793=DIRECTION('',(0.499999999999999,-0.866025403784439,0.));
#7794=DIRECTION('',(1.,2.00308613164953E-15,0.));
#7795=DIRECTION('center_axis',(-0.866025403784438,0.500000000000001,0.));
#7796=DIRECTION('ref_axis',(-0.500000000000001,-0.866025403784438,0.));
#7797=DIRECTION('',(0.500000000000001,0.866025403784438,0.));
#7798=DIRECTION('',(0.,0.,-1.));
#7799=DIRECTION('',(0.,0.,-1.));
#7800=DIRECTION('center_axis',(-0.866025403784438,-0.500000000000001,0.));
#7801=DIRECTION('ref_axis',(0.500000000000001,-0.866025403784438,0.));
#7802=DIRECTION('',(-0.500000000000001,0.866025403784438,0.));
#7803=DIRECTION('',(0.,0.,-1.));
#7804=DIRECTION('center_axis',(0.,-1.,0.));
#7805=DIRECTION('ref_axis',(0.,0.,-1.));
#7806=DIRECTION('',(-1.,0.,0.));
#7807=DIRECTION('',(0.,0.,-1.));
#7808=DIRECTION('center_axis',(0.866025403784438,-0.500000000000001,0.));
#7809=DIRECTION('ref_axis',(0.500000000000001,0.866025403784438,0.));
#7810=DIRECTION('',(-0.500000000000001,-0.866025403784438,0.));
#7811=DIRECTION('',(0.,0.,-1.));
#7812=DIRECTION('center_axis',(0.866025403784439,0.499999999999999,0.));
#7813=DIRECTION('ref_axis',(-0.499999999999999,0.866025403784439,0.));
#7814=DIRECTION('',(0.499999999999999,-0.866025403784439,0.));
#7815=DIRECTION('',(0.,0.,-1.));
#7816=DIRECTION('center_axis',(-2.00308613164953E-15,1.,0.));
#7817=DIRECTION('ref_axis',(-1.,-2.00308613164953E-15,0.));
#7818=DIRECTION('',(1.,2.00308613164953E-15,0.));
#7819=DIRECTION('center_axis',(0.,0.,1.));
#7820=DIRECTION('ref_axis',(1.,0.,0.));
#7821=DIRECTION('center_axis',(0.,0.,1.));
#7822=DIRECTION('ref_axis',(1.,0.,0.));
#7823=DIRECTION('axis',(0.,0.,1.));
#7824=DIRECTION('refdir',(1.,0.,0.));
#7825=DIRECTION('center_axis',(-1.,0.,0.));
#7826=DIRECTION('ref_axis',(0.,-2.66671190320869E-15,-1.));
#7827=DIRECTION('',(1.,0.,0.));
#7828=DIRECTION('center_axis',(1.,0.,0.));
#7829=DIRECTION('ref_axis',(0.,-2.66671190320869E-15,-1.));
#7830=DIRECTION('center_axis',(-1.,0.,0.));
#7831=DIRECTION('ref_axis',(0.,-2.66671190320869E-15,-1.));
#7832=DIRECTION('',(1.,0.,0.));
#7833=DIRECTION('center_axis',(-1.,0.,0.));
#7834=DIRECTION('ref_axis',(0.,-2.66671190320869E-15,-1.));
#7835=DIRECTION('',(1.,0.,0.));
#7836=DIRECTION('center_axis',(-1.,0.,0.));
#7837=DIRECTION('ref_axis',(0.,-2.66671190320869E-15,-1.));
#7838=DIRECTION('',(1.,0.,0.));
#7839=DIRECTION('center_axis',(-1.,0.,0.));
#7840=DIRECTION('ref_axis',(0.,-2.66671190320869E-15,-1.));
#7841=DIRECTION('center_axis',(-1.,0.,0.));
#7842=DIRECTION('ref_axis',(0.,0.,1.));
#7843=DIRECTION('',(-0.707106781186548,-8.65956056235493E-17,-0.707106781186547));
#7844=DIRECTION('center_axis',(-1.,0.,0.));
#7845=DIRECTION('ref_axis',(0.,0.,1.));
#7846=DIRECTION('center_axis',(-1.,0.,0.));
#7847=DIRECTION('ref_axis',(0.,0.,1.));
#7848=DIRECTION('center_axis',(1.,0.,0.));
#7849=DIRECTION('ref_axis',(0.,0.,-1.));
#7850=DIRECTION('',(0.707106781186548,-8.65956056235493E-17,0.707106781186547));
#7851=DIRECTION('center_axis',(-1.,0.,0.));
#7852=DIRECTION('ref_axis',(0.,0.,1.));
#7853=DIRECTION('center_axis',(-1.,0.,0.));
#7854=DIRECTION('ref_axis',(0.,0.,1.));
#7855=DIRECTION('center_axis',(-1.,0.,0.));
#7856=DIRECTION('ref_axis',(0.,0.,1.));
#7857=DIRECTION('',(-1.,0.,0.));
#7858=DIRECTION('center_axis',(-1.,0.,0.));
#7859=DIRECTION('ref_axis',(0.,0.,1.));
#7860=DIRECTION('',(-1.,0.,0.));
#7861=DIRECTION('center_axis',(-1.,0.,0.));
#7862=DIRECTION('ref_axis',(0.,0.,1.));
#7863=DIRECTION('',(-1.,0.,0.));
#7864=DIRECTION('center_axis',(-1.,0.,0.));
#7865=DIRECTION('ref_axis',(0.,0.,1.));
#7866=DIRECTION('center_axis',(1.,0.,0.));
#7867=DIRECTION('ref_axis',(0.,0.,-1.));
#7868=DIRECTION('',(-0.5,1.06057523872491E-16,-0.866025403784439));
#7869=DIRECTION('center_axis',(-1.,0.,0.));
#7870=DIRECTION('ref_axis',(0.,0.,1.));
#7871=DIRECTION('center_axis',(1.,0.,0.));
#7872=DIRECTION('ref_axis',(0.,0.,-1.));
#7873=DIRECTION('center_axis',(-1.,0.,0.));
#7874=DIRECTION('ref_axis',(0.,0.,1.));
#7875=DIRECTION('center_axis',(-1.,0.,0.));
#7876=DIRECTION('ref_axis',(0.,0.,1.));
#7877=DIRECTION('center_axis',(-1.,0.,0.));
#7878=DIRECTION('ref_axis',(0.,0.,1.));
#7879=DIRECTION('center_axis',(-1.,0.,0.));
#7880=DIRECTION('ref_axis',(0.,0.,1.));
#7881=DIRECTION('',(0.,-0.5,0.866025403784439));
#7882=DIRECTION('',(0.,-1.,0.));
#7883=DIRECTION('',(0.,-0.5,-0.866025403784439));
#7884=DIRECTION('',(0.,0.5,-0.866025403784439));
#7885=DIRECTION('',(0.,1.,0.));
#7886=DIRECTION('',(0.,0.5,0.866025403784439));
#7887=DIRECTION('center_axis',(0.999999998812523,4.82472814902002E-5,-6.86688143352015E-6));
#7888=DIRECTION('ref_axis',(-4.8541881071249E-5,0.998613318949696,-0.0526444380724065));
#7889=DIRECTION('center_axis',(0.999999999837215,-4.38888781624564E-6,1.75016240224852E-5));
#7890=DIRECTION('ref_axis',(1.79722394331351E-5,0.32841963521485,-0.944531917344429));
#7891=DIRECTION('center_axis',(1.,0.,0.));
#7892=DIRECTION('ref_axis',(0.,0.,-1.));
#7893=DIRECTION('center_axis',(-0.999999999904602,-1.36751150609827E-5,
1.94633545137007E-6));
#7894=DIRECTION('ref_axis',(-1.37586092717476E-5,0.973645618966202,-0.228066237042274));
#7895=DIRECTION('center_axis',(-0.999999999786601,5.02509006274664E-6,-2.00386156144365E-5));
#7896=DIRECTION('ref_axis',(2.05774510033662E-5,0.156136104303204,-0.9877355498865));
#7897=DIRECTION('center_axis',(0.,0.866025403784439,0.5));
#7898=DIRECTION('ref_axis',(0.,-0.5,0.866025403784439));
#7899=DIRECTION('',(1.,0.,0.));
#7900=DIRECTION('',(1.,0.,0.));
#7901=DIRECTION('center_axis',(0.,0.866025403784439,-0.5));
#7902=DIRECTION('ref_axis',(0.,0.5,0.866025403784439));
#7903=DIRECTION('',(1.,0.,0.));
#7904=DIRECTION('center_axis',(0.,0.,-1.));
#7905=DIRECTION('ref_axis',(-1.,0.,0.));
#7906=DIRECTION('',(1.,0.,0.));
#7907=DIRECTION('center_axis',(0.,-0.866025403784439,-0.5));
#7908=DIRECTION('ref_axis',(0.,0.5,-0.866025403784439));
#7909=DIRECTION('',(1.,0.,0.));
#7910=DIRECTION('center_axis',(0.,-0.866025403784439,0.5));
#7911=DIRECTION('ref_axis',(0.,-0.5,-0.866025403784439));
#7912=DIRECTION('',(1.,0.,0.));
#7913=DIRECTION('center_axis',(0.,0.,1.));
#7914=DIRECTION('ref_axis',(1.,0.,0.));
#7915=DIRECTION('center_axis',(-1.,0.,0.));
#7916=DIRECTION('ref_axis',(0.,-2.66671190320869E-15,-1.));
#7917=DIRECTION('',(0.,0.,1.));
#7918=DIRECTION('',(1.,0.,0.));
#7919=DIRECTION('',(5.57827649406208E-20,2.61263476009516E-21,-1.));
#7920=DIRECTION('',(-1.,-2.08166817117217E-17,-5.57827649406208E-20));
#7921=DIRECTION('',(0.,0.,1.));
#7922=DIRECTION('',(1.,0.,0.));
#7923=DIRECTION('',(-1.78555597446133E-17,2.36620771243881E-17,-1.));
#7924=DIRECTION('',(0.99894011039311,-0.0460288588583357,-1.89257732306683E-17));
#7925=DIRECTION('',(1.55841164283545E-15,1.64782951837159E-15,-1.));
#7926=DIRECTION('',(-0.965958930699627,-0.258695466140466,-1.93164766947834E-15));
#7927=DIRECTION('',(1.55849527171628E-15,1.64812859515955E-15,-1.));
#7928=DIRECTION('',(-0.258695466140466,0.965958930699627,1.18884887464145E-15));
#7929=DIRECTION('',(0.581306235198843,-0.813684865853451,-4.19703468239838E-16));
#7930=DIRECTION('',(-1.58650792177261E-15,-1.64922621972461E-15,1.));
#7931=DIRECTION('',(0.985808714055684,-0.16787250904147,-1.6306400674182E-16));
#7932=DIRECTION('',(1.51369882789397E-16,-8.24569628552198E-17,1.));
#7933=DIRECTION('',(0.,0.,1.));
#7934=DIRECTION('',(1.,0.,0.));
#7935=DIRECTION('',(0.,0.,1.));
#7936=DIRECTION('',(1.,0.,0.));
#7937=DIRECTION('',(-1.78555597446133E-17,2.36620771243882E-17,-1.));
#7938=DIRECTION('',(0.871107803893061,0.491091838658115,-3.93386447492551E-18));
#7939=DIRECTION('',(-1.78555597446133E-17,2.36620771243881E-17,-1.));
#7940=DIRECTION('',(0.573624094506846,-0.819118671622861,-2.96244284723831E-17));
#7941=DIRECTION('',(-1.78555597446133E-17,2.36620771243881E-17,-1.));
#7942=DIRECTION('',(0.99894011039311,-0.0460288588583357,-1.89257732306683E-17));
#7943=DIRECTION('',(0.985808714055684,-0.16787250904147,-1.6306400674182E-16));
#7944=DIRECTION('',(1.51369882789397E-16,-8.24569628552198E-17,1.));
#7945=DIRECTION('',(-0.781374182333057,-0.624062807082225,-1.74650710838922E-17));
#7946=DIRECTION('',(-1.11022302462516E-16,1.11022302462516E-16,1.));
#7947=DIRECTION('',(-0.781374182333057,-0.624062807082225,-1.74650710838922E-17));
#7948=DIRECTION('',(-1.11022302462516E-16,1.11022302462516E-16,1.));
#7949=CARTESIAN_POINT('',(0.,0.,0.));
#7950=CARTESIAN_POINT('',(0.,0.,0.));
#7951=CARTESIAN_POINT('Origin',(62.,10.,28.));
#7952=CARTESIAN_POINT('',(62.,10.,25.));
#7953=CARTESIAN_POINT('Origin',(62.,10.,28.));
#7954=CARTESIAN_POINT('',(54.,10.,25.));
#7955=CARTESIAN_POINT('',(62.,10.,25.));
#7956=CARTESIAN_POINT('Origin',(54.,10.,28.));
#7957=CARTESIAN_POINT('Origin',(62.,40.,28.));
#7958=CARTESIAN_POINT('',(62.,40.,25.));
#7959=CARTESIAN_POINT('Origin',(62.,40.,28.));
#7960=CARTESIAN_POINT('',(54.,40.,25.));
#7961=CARTESIAN_POINT('',(62.,40.,25.));
#7962=CARTESIAN_POINT('Origin',(54.,40.,28.));
#7963=CARTESIAN_POINT('Origin',(29.,24.9999999999997,2.));
#7964=CARTESIAN_POINT('',(20.5,24.9999999999997,3.));
#7965=CARTESIAN_POINT('Origin',(29.,24.9999999999997,3.));
#7966=CARTESIAN_POINT('',(20.5,24.9999999999997,5.));
#7967=CARTESIAN_POINT('',(20.5,24.9999999999997,2.));
#7968=CARTESIAN_POINT('Origin',(29.,24.9999999999997,5.));
#7969=CARTESIAN_POINT('Origin',(29.,24.9999999999997,3.));
#7970=CARTESIAN_POINT('',(38.5,24.9999999999997,3.));
#7971=CARTESIAN_POINT('Origin',(29.,24.9999999999997,3.));
#7972=CARTESIAN_POINT('',(38.5,24.9999999999997,0.));
#7973=CARTESIAN_POINT('',(38.5,24.9999999999997,3.));
#7974=CARTESIAN_POINT('Origin',(29.,24.9999999999997,0.));
#7975=CARTESIAN_POINT('Origin',(29.,24.9999999999997,5.));
#7976=CARTESIAN_POINT('',(19.5,24.9999999999997,5.));
#7977=CARTESIAN_POINT('Origin',(29.,24.9999999999997,5.));
#7978=CARTESIAN_POINT('',(19.5,24.9999999999997,8.));
#7979=CARTESIAN_POINT('',(19.5,24.9999999999997,5.));
#7980=CARTESIAN_POINT('Origin',(29.,24.9999999999997,8.));
#7981=CARTESIAN_POINT('Origin',(29.,10.,0.));
#7982=CARTESIAN_POINT('',(26.0000000000007,10.,0.));
#7983=CARTESIAN_POINT('Origin',(29.,10.,0.));
#7984=CARTESIAN_POINT('',(26.0000000000007,10.,8.));
#7985=CARTESIAN_POINT('',(26.0000000000007,10.,0.));
#7986=CARTESIAN_POINT('Origin',(29.,10.,8.));
#7987=CARTESIAN_POINT('Origin',(14.0000000000004,24.9999999999997,0.));
#7988=CARTESIAN_POINT('',(11.0000000000004,24.9999999999997,0.));
#7989=CARTESIAN_POINT('Origin',(14.0000000000004,24.9999999999997,0.));
#7990=CARTESIAN_POINT('',(11.0000000000004,24.9999999999997,8.));
#7991=CARTESIAN_POINT('',(11.0000000000004,24.9999999999997,0.));
#7992=CARTESIAN_POINT('Origin',(14.0000000000004,24.9999999999997,8.));
#7993=CARTESIAN_POINT('Origin',(44.,25.,0.));
#7994=CARTESIAN_POINT('',(41.0000000000002,25.,0.));
#7995=CARTESIAN_POINT('Origin',(44.,25.,0.));
#7996=CARTESIAN_POINT('',(41.0000000000002,25.,8.));
#7997=CARTESIAN_POINT('',(41.0000000000002,25.,0.));
#7998=CARTESIAN_POINT('Origin',(44.,25.,8.));
#7999=CARTESIAN_POINT('Origin',(29.,40.,0.));
#8000=CARTESIAN_POINT('',(26.,40.,0.));
#8001=CARTESIAN_POINT('Origin',(29.,40.,0.));
#8002=CARTESIAN_POINT('',(26.,40.,8.));
#8003=CARTESIAN_POINT('',(26.,40.,0.));
#8004=CARTESIAN_POINT('Origin',(29.,40.,8.));
#8005=CARTESIAN_POINT('Origin',(0.,0.,8.));
#8006=CARTESIAN_POINT('',(54.,50.,8.));
#8007=CARTESIAN_POINT('',(54.,-9.79717439317883E-16,8.));
#8008=CARTESIAN_POINT('',(54.,-9.79717439317883E-16,8.));
#8009=CARTESIAN_POINT('',(4.,50.,8.));
#8010=CARTESIAN_POINT('',(0.,50.,8.));
#8011=CARTESIAN_POINT('',(4.,0.,8.));
#8012=CARTESIAN_POINT('',(4.,50.,8.));
#8013=CARTESIAN_POINT('',(0.,0.,8.));
#8014=CARTESIAN_POINT('Origin',(0.,0.,0.));
#8015=CARTESIAN_POINT('',(4.,50.,0.));
#8016=CARTESIAN_POINT('',(4.,-6.93889390390723E-15,0.));
#8017=CARTESIAN_POINT('',(4.,-6.93889390390723E-17,0.));
#8018=CARTESIAN_POINT('',(62.,50.,0.));
#8019=CARTESIAN_POINT('',(0.,50.,0.));
#8020=CARTESIAN_POINT('',(62.,0.,0.));
#8021=CARTESIAN_POINT('',(62.,50.,0.));
#8022=CARTESIAN_POINT('',(0.,0.,0.));
#8023=CARTESIAN_POINT('Origin',(0.,0.,8.));
#8024=CARTESIAN_POINT('',(4.,-6.93889390390723E-15,-2.));
#8025=CARTESIAN_POINT('',(62.,0.,38.));
#8026=CARTESIAN_POINT('',(62.,0.,0.));
#8027=CARTESIAN_POINT('',(54.,-9.79717439317883E-16,38.));
#8028=CARTESIAN_POINT('',(62.,0.,38.));
#8029=CARTESIAN_POINT('',(54.,-9.79717439317883E-16,38.));
#8030=CARTESIAN_POINT('Origin',(0.,50.,8.));
#8031=CARTESIAN_POINT('',(4.,50.,-2.));
#8032=CARTESIAN_POINT('',(54.,50.,38.));
#8033=CARTESIAN_POINT('',(54.,50.,38.));
#8034=CARTESIAN_POINT('',(62.,50.,38.));
#8035=CARTESIAN_POINT('',(54.,50.,38.));
#8036=CARTESIAN_POINT('',(62.,50.,0.));
#8037=CARTESIAN_POINT('Origin',(29.,24.9999999999997,5.));
#8038=CARTESIAN_POINT('Origin',(29.,24.9999999999997,3.));
#8039=CARTESIAN_POINT('Origin',(4.,50.,-2.));
#8040=CARTESIAN_POINT('Origin',(62.,50.,0.));
#8041=CARTESIAN_POINT('',(62.,50.,38.));
#8042=CARTESIAN_POINT('Origin',(54.,-9.79717439317883E-16,38.));
#8043=CARTESIAN_POINT('',(54.,-9.79717439317883E-16,38.));
#8044=CARTESIAN_POINT('Origin',(0.,0.,38.));
#8045=CARTESIAN_POINT('',(0.,0.,0.));
#8046=CARTESIAN_POINT('Origin',(0.,0.,44.));
#8047=CARTESIAN_POINT('',(4.,-4.89858719658941E-16,34.));
#8048=CARTESIAN_POINT('Origin',(0.,0.,34.));
#8049=CARTESIAN_POINT('',(4.,-4.89858719658941E-16,44.));
#8050=CARTESIAN_POINT('',(4.,-4.89858719658941E-16,44.));
#8051=CARTESIAN_POINT('Origin',(0.,0.,44.));
#8052=CARTESIAN_POINT('Origin',(0.,0.,33.));
#8053=CARTESIAN_POINT('',(-4.24264068711928,1.5,33.));
#8054=CARTESIAN_POINT('',(-4.24264068711928,-1.5,33.));
#8055=CARTESIAN_POINT('Origin',(0.,0.,33.));
#8056=CARTESIAN_POINT('',(-4.24264068711928,-1.5,23.));
#8057=CARTESIAN_POINT('',(-4.24264068711928,-1.5,33.));
#8058=CARTESIAN_POINT('',(4.5,-5.51091059616309E-16,23.));
#8059=CARTESIAN_POINT('Origin',(0.,0.,23.));
#8060=CARTESIAN_POINT('',(4.5,-5.51091059616309E-16,34.));
#8061=CARTESIAN_POINT('',(4.5,-5.51091059616309E-16,33.));
#8062=CARTESIAN_POINT('Origin',(0.,0.,34.));
#8063=CARTESIAN_POINT('',(-4.24264068711929,1.5,23.));
#8064=CARTESIAN_POINT('Origin',(0.,0.,23.));
#8065=CARTESIAN_POINT('',(-4.24264068711929,1.5,33.));
#8066=CARTESIAN_POINT('Origin',(0.,0.,23.));
#8067=CARTESIAN_POINT('',(5.,-6.12323399573677E-16,7.));
#8068=CARTESIAN_POINT('Origin',(0.,0.,7.));
#8069=CARTESIAN_POINT('',(5.,-6.12323399573677E-16,23.));
#8070=CARTESIAN_POINT('',(5.,-6.12323399573677E-16,23.));
#8071=CARTESIAN_POINT('',(-4.76969600708473,-1.5,23.));
#8072=CARTESIAN_POINT('Origin',(0.,0.,23.));
#8073=CARTESIAN_POINT('',(-4.76969600708473,1.5,23.));
#8074=CARTESIAN_POINT('Origin',(0.,0.,23.));
#8075=CARTESIAN_POINT('Origin',(0.,0.,23.));
#8076=CARTESIAN_POINT('Origin',(0.,0.,7.));
#8077=CARTESIAN_POINT('',(6.,-7.34788079488412E-16,5.));
#8078=CARTESIAN_POINT('Origin',(0.,0.,5.));
#8079=CARTESIAN_POINT('',(6.,-7.34788079488412E-16,7.));
#8080=CARTESIAN_POINT('',(6.,-7.34788079488412E-16,7.));
#8081=CARTESIAN_POINT('Origin',(0.,0.,7.));
#8082=CARTESIAN_POINT('Origin',(0.,0.,5.));
#8083=CARTESIAN_POINT('',(5.,-6.12323399573677E-16,0.));
#8084=CARTESIAN_POINT('Origin',(0.,0.,0.));
#8085=CARTESIAN_POINT('',(5.,-6.12323399573677E-16,5.));
#8086=CARTESIAN_POINT('',(5.,-6.12323399573677E-16,5.));
#8087=CARTESIAN_POINT('Origin',(0.,0.,5.));
#8088=CARTESIAN_POINT('Origin',(0.,0.,34.));
#8089=CARTESIAN_POINT('Origin',(0.,0.,7.));
#8090=CARTESIAN_POINT('Origin',(0.,0.,0.));
#8091=CARTESIAN_POINT('Origin',(0.,0.,5.));
#8092=CARTESIAN_POINT('Origin',(0.,0.,23.));
#8093=CARTESIAN_POINT('',(-5.75,1.5,23.));
#8094=CARTESIAN_POINT('',(-5.75,-1.5,23.));
#8095=CARTESIAN_POINT('Origin',(0.,0.,23.));
#8096=CARTESIAN_POINT('',(-5.75,1.5,23.));
#8097=CARTESIAN_POINT('',(-5.75,1.5,23.));
#8098=CARTESIAN_POINT('',(-5.75,-1.5,23.));
#8099=CARTESIAN_POINT('',(-5.75,-1.5,23.));
#8100=CARTESIAN_POINT('',(-5.75,-1.53080849893419E-16,23.));
#8101=CARTESIAN_POINT('Origin',(-5.75,1.5,33.));
#8102=CARTESIAN_POINT('',(-5.75,1.5,33.));
#8103=CARTESIAN_POINT('',(-5.75,1.5,33.));
#8104=CARTESIAN_POINT('',(-5.75,1.5,33.));
#8105=CARTESIAN_POINT('Origin',(-5.75,-1.53080849893419E-16,33.));
#8106=CARTESIAN_POINT('',(-5.75,-1.5,33.));
#8107=CARTESIAN_POINT('',(-5.75,-1.5,33.));
#8108=CARTESIAN_POINT('',(-5.75,-1.53080849893419E-16,33.));
#8109=CARTESIAN_POINT('Origin',(-5.75,-1.5,33.));
#8110=CARTESIAN_POINT('',(-5.75,-1.5,33.));
#8111=CARTESIAN_POINT('Origin',(0.,0.,33.));
#8112=CARTESIAN_POINT('Origin',(0.,0.,44.));
#8113=CARTESIAN_POINT('',(0.,0.,0.));
#8114=CARTESIAN_POINT('Origin',(3.51281503885303E-14,-0.121376657232176,
-0.999999999999996));
#8115=CARTESIAN_POINT('',(-1.49999999999993,4.12126402988712,-0.999999999999996));
#8116=CARTESIAN_POINT('',(1.49999999999993,4.12126402988715,-0.999999999999996));
#8117=CARTESIAN_POINT('Origin',(3.43987251108903E-14,-0.121376657232172,
-0.999999999999996));
#8118=CARTESIAN_POINT('',(-1.49999999999993,4.12126402988712,1.));
#8119=CARTESIAN_POINT('',(-1.49999999999993,4.12126402988712,-0.999999999999996));
#8120=CARTESIAN_POINT('',(1.49999999999993,4.12126402988715,1.));
#8121=CARTESIAN_POINT('Origin',(3.43987251108903E-14,-0.121376657232172,
1.));
#8122=CARTESIAN_POINT('',(1.49999999999993,4.12126402988715,-0.999999999999996));
#8123=CARTESIAN_POINT('Origin',(3.59548358424103,18.5022254123314,-0.999999999999996));
#8124=CARTESIAN_POINT('',(3.51871169276258,18.1045684286397,1.));
#8125=CARTESIAN_POINT('',(3.19260839230423,18.5436570394041,1.));
#8126=CARTESIAN_POINT('Origin',(3.59548358424103,18.5022254123314,1.));
#8127=CARTESIAN_POINT('',(3.51871169276258,18.1045684286397,-0.999999999999996));
#8128=CARTESIAN_POINT('',(3.51871169276258,18.1045684286397,-0.999999999999996));
#8129=CARTESIAN_POINT('',(3.19260839230423,18.5436570394041,-0.999999999999996));
#8130=CARTESIAN_POINT('Origin',(3.59548358424104,18.5022254123314,-0.999999999999996));
#8131=CARTESIAN_POINT('',(3.19260839230423,18.5436570394041,-0.999999999999996));
#8132=CARTESIAN_POINT('Origin',(-2.30964438172635,19.1095079271131,-0.999999999999996));
#8133=CARTESIAN_POINT('',(2.76924223657526,21.3003715775681,-0.999999999999996));
#8134=CARTESIAN_POINT('Origin',(-2.30964438172635,19.1095079271131,-1.00000000000001));
#8135=CARTESIAN_POINT('',(2.76924223657527,21.3003715775681,1.));
#8136=CARTESIAN_POINT('',(2.76924223657526,21.3003715775681,4.082419099807E-15));
#8137=CARTESIAN_POINT('Origin',(-2.30964438172635,19.1095079271131,1.00000000000001));
#8138=CARTESIAN_POINT('Origin',(7.38897823680324,17.3477119528255,-0.999999999999996));
#8139=CARTESIAN_POINT('',(7.23120645950496,16.974706502077,1.));
#8140=CARTESIAN_POINT('',(7.0035209540531,17.4720006617853,1.));
#8141=CARTESIAN_POINT('Origin',(7.38897823680324,17.3477119528255,1.));
#8142=CARTESIAN_POINT('',(7.23120645950496,16.974706502077,-0.999999999999996));
#8143=CARTESIAN_POINT('',(7.23120645950496,16.974706502077,-0.999999999999996));
#8144=CARTESIAN_POINT('',(7.0035209540531,17.4720006617853,-0.999999999999996));
#8145=CARTESIAN_POINT('Origin',(7.38897823680324,17.3477119528255,-0.999999999999996));
#8146=CARTESIAN_POINT('',(7.0035209540531,17.4720006617853,-0.999999999999996));
#8147=CARTESIAN_POINT('Origin',(1.73915261931847,19.1694690275263,-0.999999999999996));
#8148=CARTESIAN_POINT('',(7.16255954532649,20.256497146471,-0.999999999999996));
#8149=CARTESIAN_POINT('Origin',(1.73915261931847,19.1694690275263,-1.));
#8150=CARTESIAN_POINT('',(7.1625595453265,20.256497146471,1.));
#8151=CARTESIAN_POINT('',(7.16255954532649,20.256497146471,4.082419099807E-15));
#8152=CARTESIAN_POINT('Origin',(1.73915261931844,19.1694690275263,1.00000000000001));
#8153=CARTESIAN_POINT('Origin',(3.59548358424065,-18.7449787267958,-0.999999999999996));
#8154=CARTESIAN_POINT('',(3.19260839230386,-18.7864103538685,1.));
#8155=CARTESIAN_POINT('',(3.5187116927622,-18.3473217431041,1.));
#8156=CARTESIAN_POINT('Origin',(3.59548358424064,-18.7449787267958,1.));
#8157=CARTESIAN_POINT('',(3.19260839230386,-18.7864103538685,-0.999999999999996));
#8158=CARTESIAN_POINT('',(3.19260839230386,-18.7864103538685,-0.999999999999996));
#8159=CARTESIAN_POINT('',(3.5187116927622,-18.3473217431041,-0.999999999999996));
#8160=CARTESIAN_POINT('Origin',(3.59548358424064,-18.7449787267958,-0.999999999999996));
#8161=CARTESIAN_POINT('',(3.5187116927622,-18.3473217431041,-0.999999999999996));
#8162=CARTESIAN_POINT('Origin',(-2.30964438172673,-19.3522612415774,-0.999999999999996));
#8163=CARTESIAN_POINT('',(2.76924223657483,-21.5431248920325,-0.999999999999996));
#8164=CARTESIAN_POINT('Origin',(-2.30964438172671,-19.3522612415774,-1.));
#8165=CARTESIAN_POINT('',(2.76924223657484,-21.5431248920325,1.));
#8166=CARTESIAN_POINT('Origin',(-2.30964438172672,-19.3522612415774,1.00000000000001));
#8167=CARTESIAN_POINT('',(2.76924223657483,-21.5431248920325,4.082419099807E-15));
#8168=CARTESIAN_POINT('Origin',(7.38897823680289,-17.59046526729,-0.999999999999996));
#8169=CARTESIAN_POINT('',(7.00352095405275,-17.7147539762498,1.));
#8170=CARTESIAN_POINT('',(7.23120645950461,-17.2174598165415,1.));
#8171=CARTESIAN_POINT('Origin',(7.38897823680288,-17.5904652672901,1.));
#8172=CARTESIAN_POINT('',(7.00352095405275,-17.7147539762498,-0.999999999999996));
#8173=CARTESIAN_POINT('',(7.00352095405275,-17.7147539762498,-0.999999999999996));
#8174=CARTESIAN_POINT('',(7.23120645950461,-17.2174598165415,-0.999999999999996));
#8175=CARTESIAN_POINT('Origin',(7.38897823680288,-17.59046526729,-0.999999999999996));
#8176=CARTESIAN_POINT('',(7.23120645950461,-17.2174598165415,-0.999999999999996));
#8177=CARTESIAN_POINT('Origin',(1.73915261931808,-19.4122223419907,-0.999999999999996));
#8178=CARTESIAN_POINT('',(7.16255954532608,-20.4992504609355,-0.999999999999996));
#8179=CARTESIAN_POINT('Origin',(1.73915261931809,-19.4122223419907,-1.00000000000001));
#8180=CARTESIAN_POINT('',(7.16255954532609,-20.4992504609355,1.));
#8181=CARTESIAN_POINT('Origin',(1.73915261931808,-19.4122223419907,1.00000000000001));
#8182=CARTESIAN_POINT('',(7.16255954532608,-20.4992504609355,4.082419099807E-15));
#8183=CARTESIAN_POINT('Origin',(13.8554859637,-13.0748150023093,-0.999999999999996));
#8184=CARTESIAN_POINT('',(13.5539059861828,-13.3451379890507,1.));
#8185=CARTESIAN_POINT('',(13.5596392883185,-12.7982291301724,1.));
#8186=CARTESIAN_POINT('Origin',(13.8554859637,-13.0748150023093,1.));
#8187=CARTESIAN_POINT('',(13.5539059861828,-13.3451379890507,-0.999999999999996));
#8188=CARTESIAN_POINT('',(13.5539059861828,-13.3451379890507,-0.999999999999996));
#8189=CARTESIAN_POINT('',(13.5596392883185,-12.7982291301724,-0.999999999999996));
#8190=CARTESIAN_POINT('Origin',(13.8554859637,-13.0748150023093,-0.999999999999996));
#8191=CARTESIAN_POINT('',(13.5596392883185,-12.7982291301724,-0.999999999999996));
#8192=CARTESIAN_POINT('Origin',(10.8595390841654,-15.6724688095372,-0.999999999999996));
#8193=CARTESIAN_POINT('',(10.5083460434874,-15.8741825873991,1.));
#8194=CARTESIAN_POINT('',(10.6276628047883,-15.3404170198083,1.));
#8195=CARTESIAN_POINT('Origin',(10.8595390841655,-15.6724688095372,1.));
#8196=CARTESIAN_POINT('',(10.5083460434874,-15.8741825873991,-0.999999999999996));
#8197=CARTESIAN_POINT('',(10.5083460434874,-15.8741825873991,-0.999999999999996));
#8198=CARTESIAN_POINT('',(10.6276628047883,-15.3404170198083,-0.999999999999996));
#8199=CARTESIAN_POINT('Origin',(10.8595390841655,-15.6724688095372,-0.999999999999996));
#8200=CARTESIAN_POINT('',(10.6276628047883,-15.3404170198083,-0.999999999999996));
#8201=CARTESIAN_POINT('Origin',(16.2458816206226,-9.91103378190805,-0.999999999999996));
#8202=CARTESIAN_POINT('',(16.0070951984252,-10.2381515658547,1.));
#8203=CARTESIAN_POINT('',(15.8989944685809,-9.70200195718188,1.));
#8204=CARTESIAN_POINT('Origin',(16.2458816206226,-9.91103378190806,1.));
#8205=CARTESIAN_POINT('',(16.0070951984252,-10.2381515658547,-0.999999999999996));
#8206=CARTESIAN_POINT('',(16.0070951984252,-10.2381515658547,-0.999999999999996));
#8207=CARTESIAN_POINT('',(15.8989944685809,-9.70200195718188,-0.999999999999996));
#8208=CARTESIAN_POINT('Origin',(16.2458816206226,-9.91103378190805,-0.999999999999996));
#8209=CARTESIAN_POINT('',(15.8989944685809,-9.70200195718188,-0.999999999999996));
#8210=CARTESIAN_POINT('Origin',(17.9262542943349,-6.31939756917167,-0.999999999999996));
#8211=CARTESIAN_POINT('',(17.7606975399316,-6.68901353347981,1.));
#8212=CARTESIAN_POINT('',(17.5434872987264,-6.18705548564272,1.));
#8213=CARTESIAN_POINT('Origin',(17.9262542943349,-6.31939756917167,1.));
#8214=CARTESIAN_POINT('',(17.7606975399316,-6.68901353347981,-0.999999999999996));
#8215=CARTESIAN_POINT('',(17.7606975399316,-6.68901353347981,-0.999999999999996));
#8216=CARTESIAN_POINT('',(17.5434872987264,-6.18705548564272,-0.999999999999996));
#8217=CARTESIAN_POINT('Origin',(17.9262542943349,-6.31939756917167,-0.999999999999996));
#8218=CARTESIAN_POINT('',(17.5434872987264,-6.18705548564272,-0.999999999999996));
#8219=CARTESIAN_POINT('Origin',(18.823163635673,-2.45687810117945,-0.999999999999996));
#8220=CARTESIAN_POINT('',(18.7380721736606,-2.85283825459467,1.));
#8221=CARTESIAN_POINT('',(18.4212455509255,-2.4070097429457,1.));
#8222=CARTESIAN_POINT('Origin',(18.823163635673,-2.45687810117946,1.));
#8223=CARTESIAN_POINT('',(18.7380721736606,-2.85283825459467,-0.999999999999996));
#8224=CARTESIAN_POINT('',(18.7380721736606,-2.85283825459467,-0.999999999999996));
#8225=CARTESIAN_POINT('',(18.4212455509255,-2.4070097429457,-0.999999999999996));
#8226=CARTESIAN_POINT('Origin',(18.823163635673,-2.45687810117946,-0.999999999999996));
#8227=CARTESIAN_POINT('',(18.4212455509255,-2.4070097429457,-0.999999999999996));
#8228=CARTESIAN_POINT('Origin',(18.823163635673,2.21412478671471,-0.999999999999996));
#8229=CARTESIAN_POINT('',(18.4212455509256,2.16425642848097,1.));
#8230=CARTESIAN_POINT('',(18.7380721736607,2.61008494012994,1.));
#8231=CARTESIAN_POINT('Origin',(18.823163635673,2.21412478671472,1.));
#8232=CARTESIAN_POINT('',(18.4212455509256,2.16425642848097,-0.999999999999996));
#8233=CARTESIAN_POINT('',(18.4212455509256,2.16425642848097,-0.999999999999996));
#8234=CARTESIAN_POINT('',(18.7380721736607,2.61008494012994,-0.999999999999996));
#8235=CARTESIAN_POINT('Origin',(18.823163635673,2.21412478671472,-0.999999999999996));
#8236=CARTESIAN_POINT('',(18.7380721736607,2.61008494012994,-0.999999999999996));
#8237=CARTESIAN_POINT('Origin',(13.8554859637002,12.8320616878447,-0.999999999999996));
#8238=CARTESIAN_POINT('',(13.5596392883187,12.5554758157078,1.));
#8239=CARTESIAN_POINT('',(13.5539059861831,13.102384674586,1.));
#8240=CARTESIAN_POINT('Origin',(13.8554859637002,12.8320616878447,1.));
#8241=CARTESIAN_POINT('',(13.5596392883187,12.5554758157078,-0.999999999999996));
#8242=CARTESIAN_POINT('',(13.5596392883187,12.5554758157078,-0.999999999999996));
#8243=CARTESIAN_POINT('',(13.5539059861831,13.102384674586,-0.999999999999996));
#8244=CARTESIAN_POINT('Origin',(13.8554859637002,12.8320616878447,-0.999999999999996));
#8245=CARTESIAN_POINT('',(13.5539059861831,13.102384674586,-0.999999999999996));
#8246=CARTESIAN_POINT('Origin',(10.8595390841658,15.4297154950726,-0.999999999999996));
#8247=CARTESIAN_POINT('',(10.6276628047886,15.0976637053437,1.));
#8248=CARTESIAN_POINT('',(10.5083460434877,15.6314292729346,1.));
#8249=CARTESIAN_POINT('Origin',(10.8595390841658,15.4297154950726,1.));
#8250=CARTESIAN_POINT('',(10.6276628047886,15.0976637053437,-0.999999999999996));
#8251=CARTESIAN_POINT('',(10.6276628047886,15.0976637053437,-0.999999999999996));
#8252=CARTESIAN_POINT('',(10.5083460434877,15.6314292729346,-0.999999999999996));
#8253=CARTESIAN_POINT('Origin',(10.8595390841658,15.4297154950726,-0.999999999999996));
#8254=CARTESIAN_POINT('',(10.5083460434877,15.6314292729346,-0.999999999999996));
#8255=CARTESIAN_POINT('Origin',(16.2458816206228,9.66828046744336,-0.999999999999996));
#8256=CARTESIAN_POINT('',(15.8989944685811,9.45924864271719,1.));
#8257=CARTESIAN_POINT('',(16.0070951984254,9.99539825138999,1.));
#8258=CARTESIAN_POINT('Origin',(16.2458816206228,9.66828046744336,1.));
#8259=CARTESIAN_POINT('',(15.8989944685811,9.45924864271719,-0.999999999999996));
#8260=CARTESIAN_POINT('',(15.8989944685811,9.45924864271719,-0.999999999999996));
#8261=CARTESIAN_POINT('',(16.0070951984254,9.99539825138999,-0.999999999999996));
#8262=CARTESIAN_POINT('Origin',(16.2458816206228,9.66828046744336,-0.999999999999995));
#8263=CARTESIAN_POINT('',(16.0070951984254,9.99539825138999,-0.999999999999996));
#8264=CARTESIAN_POINT('Origin',(17.9262542943351,6.07664425470695,-0.999999999999996));
#8265=CARTESIAN_POINT('',(17.5434872987265,5.944302171178,1.));
#8266=CARTESIAN_POINT('',(17.7606975399317,6.4462602190151,1.));
#8267=CARTESIAN_POINT('Origin',(17.9262542943351,6.07664425470695,1.));
#8268=CARTESIAN_POINT('',(17.5434872987265,5.944302171178,-0.999999999999996));
#8269=CARTESIAN_POINT('',(17.5434872987265,5.944302171178,-0.999999999999996));
#8270=CARTESIAN_POINT('',(17.7606975399317,6.4462602190151,-0.999999999999996));
#8271=CARTESIAN_POINT('Origin',(17.9262542943351,6.07664425470695,-0.999999999999996));
#8272=CARTESIAN_POINT('',(17.7606975399317,6.4462602190151,-0.999999999999996));
#8273=CARTESIAN_POINT('Origin',(3.64291929955129E-14,-0.121376657232174,
1.));
#8274=CARTESIAN_POINT('',(-21.5938622919806,0.393512957130182,1.));
#8275=CARTESIAN_POINT('',(-21.5938622919806,-0.636266271594385,1.));
#8276=CARTESIAN_POINT('Origin',(6.93889390390723E-12,-0.1213766572321,1.00000000000115));
#8277=CARTESIAN_POINT('',(-21.5938622919806,0.393512957130176,-0.999999999999996));
#8278=CARTESIAN_POINT('',(-21.5938622919806,0.393512957130177,4.082419099807E-15));
#8279=CARTESIAN_POINT('',(-21.5938622919806,-0.636266271594384,-0.999999999999996));
#8280=CARTESIAN_POINT('Origin',(-2.61943244872498E-12,-0.1213766572321,
-1.00000000000114));
#8281=CARTESIAN_POINT('',(-21.5938622919806,-0.636266271594385,4.082419099807E-15));
#8282=CARTESIAN_POINT('Origin',(3.64291929955129E-14,-0.121376657232174,
1.));
#8283=CARTESIAN_POINT('',(-14.831751721668,-15.8242152817228,1.));
#8284=CARTESIAN_POINT('',(-14.0664766164573,-16.5132720814551,1.));
#8285=CARTESIAN_POINT('Origin',(4.60655819045641E-12,-0.121376657226993,
1.00000000000115));
#8286=CARTESIAN_POINT('',(-14.831751721668,-15.8242152817229,-0.999999999999996));
#8287=CARTESIAN_POINT('',(-14.831751721668,-15.8242152817229,4.082419099807E-15));
#8288=CARTESIAN_POINT('',(-14.0664766164573,-16.5132720814551,-0.999999999999996));
#8289=CARTESIAN_POINT('Origin',(5.37937749900408E-12,-0.121376657226309,
-1.00000000000114));
#8290=CARTESIAN_POINT('',(-14.0664766164573,-16.5132720814551,4.082419099807E-15));
#8291=CARTESIAN_POINT('Origin',(3.64291929955129E-14,-0.121376657232174,
1.));
#8292=CARTESIAN_POINT('',(-17.7724460902854,-12.3973760042466,-0.999999999999996));
#8293=CARTESIAN_POINT('',(-17.1671570465239,-13.2304849007391,-0.999999999999996));
#8294=CARTESIAN_POINT('Origin',(1.84574577843932E-12,-0.121376657230891,
-1.00000000000114));
#8295=CARTESIAN_POINT('',(-17.1671570465239,-13.2304849007391,1.));
#8296=CARTESIAN_POINT('',(-17.1671570465239,-13.2304849007391,4.082419099807E-15));
#8297=CARTESIAN_POINT('',(-17.7724460902854,-12.3973760042466,1.));
#8298=CARTESIAN_POINT('Origin',(1.84574577843932E-12,-0.121376657230891,
1.00000000000115));
#8299=CARTESIAN_POINT('',(-17.7724460902854,-12.3973760042466,4.082419099807E-15));
#8300=CARTESIAN_POINT('Origin',(3.64291929955129E-14,-0.121376657232174,
1.));
#8301=CARTESIAN_POINT('',(-11.2428386321728,-18.5647651607291,1.));
#8302=CARTESIAN_POINT('',(-10.3510236598078,-19.0796547750914,1.));
#8303=CARTESIAN_POINT('Origin',(9.67975699595058E-13,-0.121376657230781,
1.00000000000115));
#8304=CARTESIAN_POINT('',(-11.2428386321728,-18.5647651607291,-0.999999999999996));
#8305=CARTESIAN_POINT('',(-11.2428386321728,-18.5647651607291,4.082419099807E-15));
#8306=CARTESIAN_POINT('',(-10.3510236598078,-19.0796547750914,-0.999999999999996));
#8307=CARTESIAN_POINT('Origin',(9.67975699595058E-13,-0.121376657230781,
-1.00000000000114));
#8308=CARTESIAN_POINT('',(-10.3510236598078,-19.0796547750914,4.082419099807E-15));
#8309=CARTESIAN_POINT('Origin',(3.64291929955129E-14,-0.121376657232174,
1.));
#8310=CARTESIAN_POINT('',(-7.16255954532629,-20.4992504609354,1.));
#8311=CARTESIAN_POINT('',(-6.18318129950237,-20.8174697430656,1.));
#8312=CARTESIAN_POINT('Origin',(2.8796409701215E-13,-0.121376657232032,
1.00000000000115));
#8313=CARTESIAN_POINT('',(-7.16255954532628,-20.4992504609354,-0.999999999999996));
#8314=CARTESIAN_POINT('',(-7.16255954532628,-20.4992504609354,4.082419099807E-15));
#8315=CARTESIAN_POINT('',(-6.18318129950239,-20.8174697430656,-0.999999999999996));
#8316=CARTESIAN_POINT('Origin',(1.0698907038087E-12,-0.121376657229371,
-1.00000000000114));
#8317=CARTESIAN_POINT('',(-6.18318129950239,-20.8174697430656,4.082419099807E-15));
#8318=CARTESIAN_POINT('Origin',(3.64291929955129E-14,-0.121376657232174,
1.));
#8319=CARTESIAN_POINT('',(-19.936399283099,-8.43401664852542,-0.999999999999996));
#8320=CARTESIAN_POINT('',(-19.5175503364984,-9.37476678530143,-0.999999999999996));
#8321=CARTESIAN_POINT('Origin',(4.32813507256213E-12,-0.12137665723024,
-1.00000000000114));
#8322=CARTESIAN_POINT('',(-19.5175503364984,-9.37476678530144,1.));
#8323=CARTESIAN_POINT('',(-19.5175503364984,-9.37476678530143,4.082419099807E-15));
#8324=CARTESIAN_POINT('',(-19.936399283099,-8.43401664852541,1.));
#8325=CARTESIAN_POINT('Origin',(9.83414738531252E-12,-0.121376657227855,
1.00000000000115));
#8326=CARTESIAN_POINT('',(-19.936399283099,-8.43401664852541,4.082419099807E-15));
#8327=CARTESIAN_POINT('Origin',(3.64291929955129E-14,-0.121376657232174,
1.));
#8328=CARTESIAN_POINT('',(-21.2290361617836,-4.10735503671244,-0.999999999999996));
#8329=CARTESIAN_POINT('',(-21.0149330211704,-5.11463111857488,-0.999999999999996));
#8330=CARTESIAN_POINT('Origin',(6.55378529224038E-12,-0.121376657230702,
-1.00000000000114));
#8331=CARTESIAN_POINT('',(-21.0149330211704,-5.11463111857489,1.));
#8332=CARTESIAN_POINT('',(-21.0149330211704,-5.11463111857488,4.082419099807E-15));
#8333=CARTESIAN_POINT('',(-21.2290361617836,-4.10735503671244,1.));
#8334=CARTESIAN_POINT('Origin',(6.48960052362924E-12,-0.121376657231027,
1.00000000000115));
#8335=CARTESIAN_POINT('',(-21.2290361617836,-4.10735503671244,4.082419099807E-15));
#8336=CARTESIAN_POINT('Origin',(3.64291929955129E-14,-0.121376657232174,
1.));
#8337=CARTESIAN_POINT('',(-21.0149330211704,4.87187780411067,-0.999999999999996));
#8338=CARTESIAN_POINT('',(-21.2290361617835,3.86460172224823,-0.999999999999996));
#8339=CARTESIAN_POINT('Origin',(5.27876353739742E-12,-0.121376657233244,
-1.00000000000114));
#8340=CARTESIAN_POINT('',(-21.2290361617835,3.86460172224823,1.));
#8341=CARTESIAN_POINT('',(-21.2290361617835,3.86460172224823,4.082419099807E-15));
#8342=CARTESIAN_POINT('',(-21.0149330211704,4.87187780411067,1.));
#8343=CARTESIAN_POINT('Origin',(5.9015292652731E-12,-0.12137665723334,1.00000000000115));
#8344=CARTESIAN_POINT('',(-21.0149330211704,4.87187780411067,4.082419099807E-15));
#8345=CARTESIAN_POINT('Origin',(3.64291929955129E-14,-0.121376657232174,
1.));
#8346=CARTESIAN_POINT('',(-10.3510236598076,18.8369014606271,1.));
#8347=CARTESIAN_POINT('',(-11.2428386321727,18.3220118462648,1.));
#8348=CARTESIAN_POINT('Origin',(-3.3506183938492E-12,-0.121376657226028,
1.00000000000115));
#8349=CARTESIAN_POINT('',(-10.3510236598076,18.8369014606271,-0.999999999999996));
#8350=CARTESIAN_POINT('',(-10.3510236598076,18.8369014606271,4.082419099807E-15));
#8351=CARTESIAN_POINT('',(-11.2428386321727,18.3220118462648,-0.999999999999996));
#8352=CARTESIAN_POINT('Origin',(-1.02522157430229E-12,-0.121376657230094,
-1.00000000000114));
#8353=CARTESIAN_POINT('',(-11.2428386321727,18.3220118462648,4.082419099807E-15));
#8354=CARTESIAN_POINT('Origin',(3.64291929955129E-14,-0.121376657232174,
1.));
#8355=CARTESIAN_POINT('',(-14.0664766164572,16.2705187669908,1.));
#8356=CARTESIAN_POINT('',(-14.8317517216679,15.5814619672586,1.));
#8357=CARTESIAN_POINT('Origin',(7.07246761155744E-12,-0.121376657239715,
1.00000000000115));
#8358=CARTESIAN_POINT('',(-14.0664766164572,16.2705187669908,-0.999999999999996));
#8359=CARTESIAN_POINT('',(-14.0664766164572,16.2705187669908,4.082419099807E-15));
#8360=CARTESIAN_POINT('',(-14.8317517216679,15.5814619672586,-0.999999999999996));
#8361=CARTESIAN_POINT('Origin',(2.66019845041043E-12,-0.121376657234943,
-1.00000000000114));
#8362=CARTESIAN_POINT('',(-14.8317517216679,15.5814619672586,4.082419099807E-15));
#8363=CARTESIAN_POINT('Origin',(3.64291929955129E-14,-0.121376657232174,
1.));
#8364=CARTESIAN_POINT('',(-19.5175503364983,9.13201347083722,-0.999999999999996));
#8365=CARTESIAN_POINT('',(-19.936399283099,8.1912633340612,-0.999999999999996));
#8366=CARTESIAN_POINT('Origin',(-5.58060542221739E-12,-0.121376657229723,
-1.00000000000114));
#8367=CARTESIAN_POINT('',(-19.936399283099,8.19126333406119,1.));
#8368=CARTESIAN_POINT('',(-19.936399283099,8.1912633340612,4.082419099807E-15));
#8369=CARTESIAN_POINT('',(-19.5175503364983,9.13201347083722,1.));
#8370=CARTESIAN_POINT('Origin',(1.84921522539128E-12,-0.12137665723286,
1.00000000000115));
#8371=CARTESIAN_POINT('',(-19.5175503364983,9.13201347083722,4.082419099807E-15));
#8372=CARTESIAN_POINT('Origin',(3.64291929955129E-14,-0.121376657232174,
1.));
#8373=CARTESIAN_POINT('',(-17.1671570465239,12.9877315862749,-0.999999999999996));
#8374=CARTESIAN_POINT('',(-17.7724460902853,12.1546226897824,-0.999999999999996));
#8375=CARTESIAN_POINT('Origin',(1.38951350425742E-12,-0.121376657233194,
-1.00000000000114));
#8376=CARTESIAN_POINT('',(-17.7724460902853,12.1546226897824,1.));
#8377=CARTESIAN_POINT('',(-17.7724460902853,12.1546226897824,4.082419099807E-15));
#8378=CARTESIAN_POINT('',(-17.1671570465239,12.9877315862749,1.));
#8379=CARTESIAN_POINT('Origin',(-1.54737334057131E-12,-0.121376657230937,
1.00000000000115));
#8380=CARTESIAN_POINT('',(-17.1671570465239,12.9877315862749,4.082419099807E-15));
#8381=CARTESIAN_POINT('Origin',(3.64291929955129E-14,-0.121376657232174,
1.));
#8382=CARTESIAN_POINT('',(-6.18318129950226,20.5747164286013,-0.999999999999996));
#8383=CARTESIAN_POINT('',(-7.16255954532614,20.2564971464711,-0.999999999999996));
#8384=CARTESIAN_POINT('Origin',(1.00440489259057E-12,-0.121376657234216,
-1.00000000000114));
#8385=CARTESIAN_POINT('',(-7.16255954532614,20.2564971464711,1.));
#8386=CARTESIAN_POINT('',(-7.16255954532614,20.2564971464711,4.082419099807E-15));
#8387=CARTESIAN_POINT('',(-6.18318129950225,20.5747164286013,1.));
#8388=CARTESIAN_POINT('Origin',(-2.04263689296269E-13,-0.121376657230938,
1.00000000000115));
#8389=CARTESIAN_POINT('',(-6.18318129950226,20.5747164286013,4.082419099807E-15));
#8390=CARTESIAN_POINT('Origin',(3.64291929955129E-14,-0.121376657232174,
1.));
#8391=CARTESIAN_POINT('',(-1.74510424621302,21.4080128178516,-0.999999999999996));
#8392=CARTESIAN_POINT('',(-2.7692422365749,21.3003715775681,-0.999999999999996));
#8393=CARTESIAN_POINT('Origin',(1.26483025442159E-12,-0.121376657242586,
-1.00000000000114));
#8394=CARTESIAN_POINT('',(-2.7692422365749,21.3003715775681,1.));
#8395=CARTESIAN_POINT('',(-2.7692422365749,21.3003715775681,4.082419099807E-15));
#8396=CARTESIAN_POINT('',(-1.74510424621301,21.4080128178516,1.));
#8397=CARTESIAN_POINT('Origin',(1.26331237138011E-12,-0.121376657242524,
1.00000000000115));
#8398=CARTESIAN_POINT('',(-1.74510424621302,21.4080128178516,4.082419099807E-15));
#8399=CARTESIAN_POINT('Origin',(3.64291929955129E-14,-0.121376657232174,
1.));
#8400=CARTESIAN_POINT('',(1.74510424621309,21.4080128178516,-0.999999999999996));
#8401=CARTESIAN_POINT('Origin',(-4.11996825544492E-14,-0.121376657231786,
-1.00000000000114));
#8402=CARTESIAN_POINT('',(1.74510424621309,21.4080128178516,1.));
#8403=CARTESIAN_POINT('',(1.74510424621309,21.4080128178516,4.082419099807E-15));
#8404=CARTESIAN_POINT('Origin',(-4.26525134655797E-13,-0.121376657236744,
1.00000000000115));
#8405=CARTESIAN_POINT('Origin',(3.64291929955129E-14,-0.121376657232174,
1.));
#8406=CARTESIAN_POINT('',(6.18318129950261,20.5747164286012,-0.999999999999996));
#8407=CARTESIAN_POINT('Origin',(-7.04297731246584E-13,-0.121376657234403,
-1.00000000000114));
#8408=CARTESIAN_POINT('',(6.18318129950261,20.5747164286012,1.));
#8409=CARTESIAN_POINT('',(6.18318129950261,20.5747164286012,4.082419099807E-15));
#8410=CARTESIAN_POINT('Origin',(5.85469173142172E-13,-0.121376657230185,
1.00000000000115));
#8411=CARTESIAN_POINT('Origin',(3.64291929955129E-14,-0.121376657232174,
1.));
#8412=CARTESIAN_POINT('',(6.18318129950219,-20.8174697430657,1.));
#8413=CARTESIAN_POINT('Origin',(2.9620403352304E-13,-0.121376657232835,
1.00000000000115));
#8414=CARTESIAN_POINT('',(6.18318129950219,-20.8174697430657,-0.999999999999996));
#8415=CARTESIAN_POINT('',(6.18318129950219,-20.8174697430657,4.082419099807E-15));
#8416=CARTESIAN_POINT('Origin',(-8.15753714578094E-13,-0.12137665722947,
-1.00000000000114));
#8417=CARTESIAN_POINT('Origin',(3.64291929955129E-14,-0.121376657232174,
1.));
#8418=CARTESIAN_POINT('',(10.3510236598076,-19.0796547750915,1.));
#8419=CARTESIAN_POINT('',(11.2428386321726,-18.5647651607292,1.));
#8420=CARTESIAN_POINT('Origin',(-7.0082828429463E-13,-0.12137665723075,
1.00000000000115));
#8421=CARTESIAN_POINT('',(10.3510236598076,-19.0796547750915,-0.999999999999996));
#8422=CARTESIAN_POINT('',(10.3510236598076,-19.0796547750915,4.082419099807E-15));
#8423=CARTESIAN_POINT('',(11.2428386321726,-18.5647651607292,-0.999999999999996));
#8424=CARTESIAN_POINT('Origin',(-3.07046055247895E-13,-0.121376657231387,
-1.00000000000114));
#8425=CARTESIAN_POINT('',(11.2428386321726,-18.5647651607292,4.082419099807E-15));
#8426=CARTESIAN_POINT('Origin',(3.64291929955129E-14,-0.121376657232174,
1.));
#8427=CARTESIAN_POINT('',(17.1671570465238,-13.2304849007394,1.));
#8428=CARTESIAN_POINT('',(17.7724460902853,-12.3973760042469,1.));
#8429=CARTESIAN_POINT('Origin',(7.65013052905772E-13,-0.121376657232576,
1.00000000000115));
#8430=CARTESIAN_POINT('',(17.1671570465238,-13.2304849007394,-0.999999999999996));
#8431=CARTESIAN_POINT('',(17.1671570465238,-13.2304849007394,4.082419099807E-15));
#8432=CARTESIAN_POINT('',(17.7724460902853,-12.3973760042469,-0.999999999999996));
#8433=CARTESIAN_POINT('Origin',(-2.69922972861991E-12,-0.121376657230187,
-1.00000000000114));
#8434=CARTESIAN_POINT('',(17.7724460902853,-12.3973760042469,4.082419099807E-15));
#8435=CARTESIAN_POINT('Origin',(3.64291929955129E-14,-0.121376657232174,
1.));
#8436=CARTESIAN_POINT('',(14.0664766164571,-16.5132720814553,-0.999999999999996));
#8437=CARTESIAN_POINT('',(14.8317517216679,-15.8242152817231,-0.999999999999996));
#8438=CARTESIAN_POINT('Origin',(-4.8017145815038E-12,-0.121376657226941,
-1.00000000000114));
#8439=CARTESIAN_POINT('',(14.8317517216679,-15.8242152817231,1.));
#8440=CARTESIAN_POINT('',(14.8317517216679,-15.8242152817231,4.082419099807E-15));
#8441=CARTESIAN_POINT('',(14.0664766164571,-16.5132720814553,1.));
#8442=CARTESIAN_POINT('Origin',(-3.74526798463393E-12,-0.121376657228061,
1.00000000000115));
#8443=CARTESIAN_POINT('',(14.0664766164571,-16.5132720814553,4.082419099807E-15));
#8444=CARTESIAN_POINT('Origin',(3.64291929955129E-14,-0.121376657232174,
1.));
#8445=CARTESIAN_POINT('',(19.5175503364983,-9.37476678530171,1.));
#8446=CARTESIAN_POINT('',(19.936399283099,-8.43401664852567,1.));
#8447=CARTESIAN_POINT('Origin',(-1.16746889933239E-12,-0.121376657231723,
1.00000000000115));
#8448=CARTESIAN_POINT('',(19.5175503364983,-9.37476678530171,-0.999999999999996));
#8449=CARTESIAN_POINT('',(19.5175503364983,-9.37476678530171,4.082419099807E-15));
#8450=CARTESIAN_POINT('',(19.936399283099,-8.43401664852568,-0.999999999999996));
#8451=CARTESIAN_POINT('Origin',(-3.51108031537706E-12,-0.121376657230407,
-1.00000000000114));
#8452=CARTESIAN_POINT('',(19.936399283099,-8.43401664852568,4.082419099807E-15));
#8453=CARTESIAN_POINT('Origin',(3.64291929955129E-14,-0.121376657232174,
1.));
#8454=CARTESIAN_POINT('',(21.0149330211704,-5.11463111857516,1.));
#8455=CARTESIAN_POINT('',(21.2290361617836,-4.10735503671271,1.));
#8456=CARTESIAN_POINT('Origin',(-1.57339419271096E-12,-0.121376657231742,
1.00000000000115));
#8457=CARTESIAN_POINT('',(21.0149330211704,-5.11463111857515,-0.999999999999996));
#8458=CARTESIAN_POINT('',(21.0149330211704,-5.11463111857516,4.082419099807E-15));
#8459=CARTESIAN_POINT('',(21.2290361617836,-4.10735503671272,-0.999999999999996));
#8460=CARTESIAN_POINT('Origin',(-5.76622083414691E-12,-0.121376657230946,
-1.00000000000114));
#8461=CARTESIAN_POINT('',(21.2290361617836,-4.10735503671272,4.082419099807E-15));
#8462=CARTESIAN_POINT('Origin',(3.64291929955129E-14,-0.121376657232174,
1.));
#8463=CARTESIAN_POINT('',(21.5938622919806,-0.636266271594677,1.));
#8464=CARTESIAN_POINT('',(21.5938622919806,0.393512957129885,1.));
#8465=CARTESIAN_POINT('Origin',(2.78770062589473E-12,-0.121376657232179,
1.00000000000115));
#8466=CARTESIAN_POINT('',(21.5938622919806,-0.636266271594671,-0.999999999999996));
#8467=CARTESIAN_POINT('',(21.5938622919806,-0.636266271594672,4.082419099807E-15));
#8468=CARTESIAN_POINT('',(21.5938622919806,0.393512957129885,-0.999999999999996));
#8469=CARTESIAN_POINT('Origin',(2.78770062589473E-12,-0.121376657232179,
-1.00000000000114));
#8470=CARTESIAN_POINT('',(21.5938622919806,0.393512957129885,4.082419099807E-15));
#8471=CARTESIAN_POINT('Origin',(3.64291929955129E-14,-0.121376657232174,
1.));
#8472=CARTESIAN_POINT('',(21.2290361617837,3.86460172224794,1.));
#8473=CARTESIAN_POINT('',(21.0149330211705,4.87187780411038,1.));
#8474=CARTESIAN_POINT('Origin',(3.40526218334247E-12,-0.121376657231491,
1.00000000000115));
#8475=CARTESIAN_POINT('',(21.2290361617837,3.86460172224794,-0.999999999999996));
#8476=CARTESIAN_POINT('',(21.2290361617837,3.86460172224794,4.082419099807E-15));
#8477=CARTESIAN_POINT('',(21.0149330211705,4.87187780411038,-0.999999999999996));
#8478=CARTESIAN_POINT('Origin',(3.37403716077489E-12,-0.121376657231511,
-1.00000000000114));
#8479=CARTESIAN_POINT('',(21.0149330211705,4.87187780411038,4.082419099807E-15));
#8480=CARTESIAN_POINT('Origin',(3.64291929955129E-14,-0.121376657232174,
1.));
#8481=CARTESIAN_POINT('',(14.8317517216682,15.5814619672584,1.));
#8482=CARTESIAN_POINT('',(14.0664766164575,16.2705187669906,1.));
#8483=CARTESIAN_POINT('Origin',(6.18428919185732E-13,-0.121376657231304,
1.00000000000115));
#8484=CARTESIAN_POINT('',(14.8317517216682,15.5814619672584,-0.999999999999996));
#8485=CARTESIAN_POINT('',(14.8317517216682,15.5814619672584,4.082419099807E-15));
#8486=CARTESIAN_POINT('',(14.0664766164575,16.2705187669906,-0.999999999999996));
#8487=CARTESIAN_POINT('Origin',(-4.92227786308419E-12,-0.121376657237505,
-1.00000000000114));
#8488=CARTESIAN_POINT('',(14.0664766164575,16.2705187669906,4.082419099807E-15));
#8489=CARTESIAN_POINT('Origin',(3.64291929955129E-14,-0.121376657232174,
1.));
#8490=CARTESIAN_POINT('',(11.242838632173,18.3220118462647,-0.999999999999996));
#8491=CARTESIAN_POINT('',(10.351023659808,18.836901460627,-0.999999999999996));
#8492=CARTESIAN_POINT('Origin',(-6.7394007041699E-13,-0.12137665723334,
-1.00000000000114));
#8493=CARTESIAN_POINT('',(10.351023659808,18.836901460627,1.));
#8494=CARTESIAN_POINT('',(10.351023659808,18.836901460627,4.082419099807E-15));
#8495=CARTESIAN_POINT('',(11.242838632173,18.3220118462647,1.));
#8496=CARTESIAN_POINT('Origin',(-1.03302782994419E-12,-0.121376657233805,
1.00000000000115));
#8497=CARTESIAN_POINT('',(11.242838632173,18.3220118462647,4.082419099807E-15));
#8498=CARTESIAN_POINT('Origin',(3.64291929955129E-14,-0.121376657232174,
1.));
#8499=CARTESIAN_POINT('',(17.7724460902855,12.1546226897822,-0.999999999999996));
#8500=CARTESIAN_POINT('',(17.1671570465241,12.9877315862747,-0.999999999999996));
#8501=CARTESIAN_POINT('Origin',(-4.61956861652624E-12,-0.121376657235823,
-1.00000000000114));
#8502=CARTESIAN_POINT('',(17.1671570465241,12.9877315862747,1.));
#8503=CARTESIAN_POINT('',(17.1671570465241,12.9877315862747,4.082419099807E-15));
#8504=CARTESIAN_POINT('',(17.7724460902855,12.1546226897822,1.));
#8505=CARTESIAN_POINT('Origin',(-4.1286418728248E-12,-0.121376657235486,
1.00000000000115));
#8506=CARTESIAN_POINT('',(17.7724460902855,12.1546226897822,4.082419099807E-15));
#8507=CARTESIAN_POINT('Origin',(3.64291929955129E-14,-0.121376657232174,
1.));
#8508=CARTESIAN_POINT('',(19.9363992830991,8.19126333406092,-0.999999999999996));
#8509=CARTESIAN_POINT('',(19.5175503364985,9.13201347083695,-0.999999999999996));
#8510=CARTESIAN_POINT('Origin',(-1.92380833485828E-12,-0.121376657233156,
-1.00000000000114));
#8511=CARTESIAN_POINT('',(19.5175503364985,9.13201347083695,1.));
#8512=CARTESIAN_POINT('',(19.5175503364985,9.13201347083695,4.082419099807E-15));
#8513=CARTESIAN_POINT('',(19.9363992830991,8.19126333406092,1.));
#8514=CARTESIAN_POINT('Origin',(-3.03403135948344E-12,-0.121376657233847,
1.00000000000115));
#8515=CARTESIAN_POINT('',(19.9363992830991,8.19126333406092,4.082419099807E-15));
#8516=CARTESIAN_POINT('Origin',(3.64291929955129E-14,-0.121376657232174,
1.));
#8517=CARTESIAN_POINT('',(-2.76924223657505,-21.5431248920325,1.));
#8518=CARTESIAN_POINT('',(-1.74510424621302,-21.650766132316,1.));
#8519=CARTESIAN_POINT('Origin',(-2.18683578190326E-13,-0.121376657234204,
1.00000000000115));
#8520=CARTESIAN_POINT('',(-2.76924223657505,-21.5431248920325,-0.999999999999996));
#8521=CARTESIAN_POINT('',(-2.76924223657505,-21.5431248920325,4.082419099807E-15));
#8522=CARTESIAN_POINT('',(-1.74510424621302,-21.650766132316,-0.999999999999996));
#8523=CARTESIAN_POINT('Origin',(-2.18683578190326E-13,-0.121376657234204,
-1.00000000000114));
#8524=CARTESIAN_POINT('',(-1.74510424621302,-21.650766132316,4.082419099807E-15));
#8525=CARTESIAN_POINT('Origin',(3.55704336920074E-14,-0.121376657232177,
-0.999999999999996));
#8526=CARTESIAN_POINT('',(-13.5539059861829,-13.3451379890505,-0.999999999999996));
#8527=CARTESIAN_POINT('Origin',(-9.43508879143737,-17.0370640084497,-1.00000000000001));
#8528=CARTESIAN_POINT('',(-13.5596392883186,-12.7982291301722,-0.999999999999996));
#8529=CARTESIAN_POINT('Origin',(-13.8554859637001,-13.0748150023091,-0.999999999999996));
#8530=CARTESIAN_POINT('',(-14.024775605964,-12.2816429146937,-0.999999999999996));
#8531=CARTESIAN_POINT('Origin',(-8.74300631892311E-13,-0.121376657233123,
-0.999999999999996));
#8532=CARTESIAN_POINT('',(-14.5680891476276,-12.218773477621,-0.999999999999996));
#8533=CARTESIAN_POINT('Origin',(-14.3307707100941,-12.5469578148565,-0.999999999999996));
#8534=CARTESIAN_POINT('Origin',(-17.8092567781527,-7.73660824112161,-0.999999999999996));
#8535=CARTESIAN_POINT('',(-16.0070951984253,-10.2381515658545,-0.999999999999996));
#8536=CARTESIAN_POINT('Origin',(-12.7458786225912,-14.7057503909453,-1.));
#8537=CARTESIAN_POINT('',(-15.8989944685809,-9.70200195718166,-0.999999999999996));
#8538=CARTESIAN_POINT('Origin',(-16.2458816206227,-9.91103378190783,-0.999999999999996));
#8539=CARTESIAN_POINT('',(-16.2465621281866,-9.09999711167674,-0.999999999999996));
#8540=CARTESIAN_POINT('Origin',(-2.48412401759879E-12,-0.121376657233779,
-0.999999999999996));
#8541=CARTESIAN_POINT('',(-16.7649316744485,-8.92554028555318,-0.999999999999996));
#8542=CARTESIAN_POINT('Origin',(-16.6010325746198,-9.29589428522826,-0.999999999999995));
#8543=CARTESIAN_POINT('Origin',(-19.0033774629777,-3.86744447109249,-1.00000000000001));
#8544=CARTESIAN_POINT('',(-17.7606975399316,-6.68901353347958,-0.999999999999996));
#8545=CARTESIAN_POINT('Origin',(-15.4996123964263,-11.7370296576879,-1.));
#8546=CARTESIAN_POINT('',(-17.5434872987264,-6.18705548564248,-0.999999999999996));
#8547=CARTESIAN_POINT('Origin',(-17.926254294335,-6.31939756917143,-0.999999999999996));
#8548=CARTESIAN_POINT('',(-17.758295925753,-5.52594251059953,-0.999999999999996));
#8549=CARTESIAN_POINT('Origin',(9.73179870022989E-13,-0.121376657231793,
-0.999999999999996));
#8550=CARTESIAN_POINT('',(-18.2290662400285,-5.24752289586338,-0.999999999999996));
#8551=CARTESIAN_POINT('Origin',(-18.1457496550421,-5.64386031103663,-0.999999999999996));
#8552=CARTESIAN_POINT('Origin',(-19.3669593643481,0.165440438030001,-1.));
#8553=CARTESIAN_POINT('',(-18.7380721736606,-2.85283825459442,-0.999999999999996));
#8554=CARTESIAN_POINT('Origin',(-17.5759387331454,-8.26064915022346,-0.999999999999996));
#8555=CARTESIAN_POINT('',(-18.4212455509255,-2.40700974294545,-0.999999999999996));
#8556=CARTESIAN_POINT('Origin',(-18.8231636356729,-2.45687810117919,-0.999999999999995));
#8557=CARTESIAN_POINT('',(-18.4939069776057,-1.71568244774586,-0.999999999999996));
#8558=CARTESIAN_POINT('Origin',(3.52669282666085E-12,-0.121376657231728,
-0.999999999999996));
#8559=CARTESIAN_POINT('',(-18.8965031381544,-1.34546831756664,-0.999999999999996));
#8560=CARTESIAN_POINT('Origin',(-18.8974104025717,-1.75046730135707,-0.999999999999995));
#8561=CARTESIAN_POINT('Origin',(-18.8841122085148,4.18579006378843,-1.));
#8562=CARTESIAN_POINT('',(-18.8965031381544,1.10271500310242,-0.999999999999996));
#8563=CARTESIAN_POINT('Origin',(-18.8841122085149,-4.42854337825268,-0.999999999999996));
#8564=CARTESIAN_POINT('',(-18.4939069776057,1.47292913328164,-0.999999999999996));
#8565=CARTESIAN_POINT('Origin',(-18.8974104025716,1.50771398689285,-0.999999999999996));
#8566=CARTESIAN_POINT('',(-18.4212455509255,2.16425642848123,-0.999999999999996));
#8567=CARTESIAN_POINT('Origin',(-3.32199545649559E-12,-0.121376657231894,
-0.999999999999996));
#8568=CARTESIAN_POINT('',(-18.7380721736606,2.61008494013019,-0.999999999999996));
#8569=CARTESIAN_POINT('Origin',(-18.8231636356729,2.21412478671497,-0.999999999999996));
#8570=CARTESIAN_POINT('Origin',(-17.5759387331454,8.01789583575931,-1.00000000000001));
#8571=CARTESIAN_POINT('',(-18.2290662400284,5.00476958139915,-0.999999999999996));
#8572=CARTESIAN_POINT('Origin',(-19.3669593643482,-0.408193752494279,-1.00000000000001));
#8573=CARTESIAN_POINT('',(-17.7582959257529,5.2831891961353,-0.999999999999996));
#8574=CARTESIAN_POINT('Origin',(-18.1457496550421,5.40110699657241,-0.999999999999996));
#8575=CARTESIAN_POINT('',(-17.5434872987263,5.94430217117825,-0.999999999999996));
#8576=CARTESIAN_POINT('Origin',(7.0082828429463E-13,-0.121376657232305,
-0.999999999999996));
#8577=CARTESIAN_POINT('',(-17.7606975399316,6.44626021901535,-0.999999999999996));
#8578=CARTESIAN_POINT('Origin',(-17.9262542943349,6.0766442547072,-0.999999999999996));
#8579=CARTESIAN_POINT('Origin',(-15.4996123964262,11.4942763432237,-1.00000000000001));
#8580=CARTESIAN_POINT('',(-16.7649316744485,8.68278697108894,-0.999999999999996));
#8581=CARTESIAN_POINT('Origin',(-19.0033774629776,3.62469115662824,-1.00000000000001));
#8582=CARTESIAN_POINT('',(-16.2465621281866,8.85724379721251,-0.999999999999996));
#8583=CARTESIAN_POINT('Origin',(-16.6010325746197,9.05314097076402,-0.999999999999996));
#8584=CARTESIAN_POINT('',(-15.8989944685809,9.45924864271742,-0.999999999999996));
#8585=CARTESIAN_POINT('Origin',(3.8372083288607E-12,-0.121376657234332,
-0.999999999999996));
#8586=CARTESIAN_POINT('',(-16.0070951984252,9.99539825139022,-0.999999999999996));
#8587=CARTESIAN_POINT('Origin',(-16.2458816206226,9.66828046744359,-0.999999999999996));
#8588=CARTESIAN_POINT('Origin',(-12.7458786225911,14.462997076481,-1.));
#8589=CARTESIAN_POINT('',(-14.5680891476275,11.9760201631568,-0.999999999999996));
#8590=CARTESIAN_POINT('Origin',(-17.8092567781527,7.49385492665739,-1.00000000000001));
#8591=CARTESIAN_POINT('',(-14.0247756059639,12.0388896002294,-0.999999999999996));
#8592=CARTESIAN_POINT('Origin',(-14.330770710094,12.3042045003922,-0.999999999999996));
#8593=CARTESIAN_POINT('',(-13.5596392883185,12.555475815708,-0.999999999999996));
#8594=CARTESIAN_POINT('Origin',(1.06442632485937E-11,-0.1213766572417,-0.999999999999996));
#8595=CARTESIAN_POINT('',(-13.5539059861829,13.1023846745862,-0.999999999999996));
#8596=CARTESIAN_POINT('Origin',(-13.8554859637,12.8320616878448,-0.999999999999995));
#8597=CARTESIAN_POINT('Origin',(-9.43508879143732,16.7943106939854,-1.));
#8598=CARTESIAN_POINT('',(-11.7345512196076,14.7405390644231,-0.999999999999996));
#8599=CARTESIAN_POINT('Origin',(-15.8367861138271,11.030196534535,-1.00000000000001));
#8600=CARTESIAN_POINT('',(-11.1900390914206,14.6890734163638,-0.999999999999996));
#8601=CARTESIAN_POINT('Origin',(-11.4341853988698,15.0122105088786,-0.999999999999996));
#8602=CARTESIAN_POINT('',(-10.6276628047883,15.0976637053439,-0.999999999999996));
#8603=CARTESIAN_POINT('Origin',(-9.26342336171615E-13,-0.121376657230733,
-0.999999999999996));
#8604=CARTESIAN_POINT('',(-10.5083460434875,15.6314292729347,-0.999999999999996));
#8605=CARTESIAN_POINT('Origin',(-10.8595390841655,15.4297154950728,-0.999999999999996));
#8606=CARTESIAN_POINT('Origin',(-5.71194030551858,18.3863276037679,-1.));
#8607=CARTESIAN_POINT('',(-8.38815709466669,16.8555209332692,-0.999999999999996));
#8608=CARTESIAN_POINT('Origin',(-13.1721719029961,14.0791608827473,-1.00000000000001));
#8609=CARTESIAN_POINT('',(-7.8662441728172,16.6919694958576,-0.999999999999996));
#8610=CARTESIAN_POINT('Origin',(-8.03787131840593,17.0588061391977,-0.999999999999996));
#8611=CARTESIAN_POINT('',(-7.23120645950465,16.9747065020771,-0.999999999999996));
#8612=CARTESIAN_POINT('Origin',(5.46524631106493E-12,-0.12137665724324,
-0.999999999999996));
#8613=CARTESIAN_POINT('',(-7.0035209540528,17.4720006617854,-0.999999999999996));
#8614=CARTESIAN_POINT('Origin',(-7.38897823680293,17.3477119528257,-0.999999999999996));
#8615=CARTESIAN_POINT('Origin',(-1.73915261931814,19.1694690275264,-0.999999999999996));
#8616=CARTESIAN_POINT('',(-4.67516025384538,18.2285309132174,-0.999999999999996));
#8617=CARTESIAN_POINT('Origin',(-9.93187057291064,16.5074935987233,-0.999999999999996));
#8618=CARTESIAN_POINT('',(-4.19865663743425,17.9600416690753,-0.999999999999996));
#8619=CARTESIAN_POINT('Origin',(-4.29026369134191,18.3545453416493,-0.999999999999996));
#8620=CARTESIAN_POINT('',(-3.51871169276225,18.1045684286397,-0.999999999999996));
#8621=CARTESIAN_POINT('Origin',(1.46844342241437E-12,-0.121376657238497,
-0.999999999999996));
#8622=CARTESIAN_POINT('',(-3.19260839230391,18.5436570394042,-0.999999999999996));
#8623=CARTESIAN_POINT('Origin',(-3.5954835842407,18.5022254123315,-0.999999999999996));
#8624=CARTESIAN_POINT('Origin',(2.30964438172666,19.109507927113,-1.));
#8625=CARTESIAN_POINT('',(-0.757836476023246,18.7995618797112,-0.999999999999996));
#8626=CARTESIAN_POINT('Origin',(-6.25749884038649,18.2090648903413,-1.00000000000001));
#8627=CARTESIAN_POINT('',(-0.347567659605682,18.4378690971619,-0.999999999999996));
#8628=CARTESIAN_POINT('Origin',(-0.35515095399708,18.8427980954396,-0.999999999999996));
#8629=CARTESIAN_POINT('',(0.347567659605759,18.4378690971619,-0.999999999999996));
#8630=CARTESIAN_POINT('Origin',(3.74591850593742E-14,-0.121376657224663,
-0.999999999999996));
#8631=CARTESIAN_POINT('',(0.757836476023318,18.7995618797112,-0.999999999999996));
#8632=CARTESIAN_POINT('Origin',(0.35515095399715,18.8427980954396,-0.999999999999996));
#8633=CARTESIAN_POINT('Origin',(6.25749884038657,18.2090648903413,-1.00000000000001));
#8634=CARTESIAN_POINT('',(4.19865663743457,17.9600416690753,-0.999999999999996));
#8635=CARTESIAN_POINT('Origin',(-1.20715069884536E-12,-0.121376657237335,
-0.999999999999996));
#8636=CARTESIAN_POINT('',(4.6751602538457,18.2285309132174,-0.999999999999996));
#8637=CARTESIAN_POINT('Origin',(4.29026369134224,18.3545453416493,-0.999999999999996));
#8638=CARTESIAN_POINT('Origin',(9.93187057291089,16.5074935987231,-1.));
#8639=CARTESIAN_POINT('',(7.8662441728175,16.6919694958575,-0.999999999999996));
#8640=CARTESIAN_POINT('Origin',(-4.48686227061401E-12,-0.121376657241696,
-0.999999999999996));
#8641=CARTESIAN_POINT('',(8.38815709466699,16.8555209332691,-0.999999999999996));
#8642=CARTESIAN_POINT('Origin',(8.03787131840625,17.0588061391976,-0.999999999999996));
#8643=CARTESIAN_POINT('Origin',(13.1721719029964,14.0791608827472,-1.));
#8644=CARTESIAN_POINT('Origin',(5.71194030551892,18.3863276037678,-1.00000000000001));
#8645=CARTESIAN_POINT('',(11.1900390914209,14.6890734163636,-0.999999999999996));
#8646=CARTESIAN_POINT('Origin',(2.03656536079677E-12,-0.121376657229092,
-0.999999999999996));
#8647=CARTESIAN_POINT('',(11.7345512196078,14.740539064423,-0.999999999999996));
#8648=CARTESIAN_POINT('Origin',(11.4341853988701,15.0122105088784,-0.999999999999996));
#8649=CARTESIAN_POINT('Origin',(15.8367861138273,11.0301965345349,-0.999999999999996));
#8650=CARTESIAN_POINT('Origin',(9.43508879143763,16.7943106939853,-1.));
#8651=CARTESIAN_POINT('',(14.0247756059641,12.0388896002292,-0.999999999999996));
#8652=CARTESIAN_POINT('Origin',(-1.08160008727154E-12,-0.121376657233035,
-0.999999999999996));
#8653=CARTESIAN_POINT('',(14.5680891476277,11.9760201631566,-0.999999999999996));
#8654=CARTESIAN_POINT('Origin',(14.3307707100943,12.304204500392,-0.999999999999996));
#8655=CARTESIAN_POINT('Origin',(17.8092567781528,7.49385492665722,-0.999999999999996));
#8656=CARTESIAN_POINT('Origin',(12.7458786225913,14.4629970764809,-1.00000000000001));
#8657=CARTESIAN_POINT('',(16.2465621281868,8.85724379721227,-0.999999999999996));
#8658=CARTESIAN_POINT('Origin',(-2.16666962149503E-12,-0.121376657233593,
-0.999999999999996));
#8659=CARTESIAN_POINT('',(16.7649316744487,8.68278697108871,-0.999999999999996));
#8660=CARTESIAN_POINT('Origin',(16.6010325746199,9.05314097076378,-0.999999999999996));
#8661=CARTESIAN_POINT('Origin',(19.0033774629777,3.62469115662801,-1.00000000000001));
#8662=CARTESIAN_POINT('Origin',(15.4996123964264,11.4942763432235,-0.999999999999996));
#8663=CARTESIAN_POINT('',(17.7582959257531,5.28318919613505,-0.999999999999996));
#8664=CARTESIAN_POINT('Origin',(-2.30544749957318E-12,-0.121376657233087,
-0.999999999999996));
#8665=CARTESIAN_POINT('',(18.2290662400286,5.0047695813989,-0.999999999999996));
#8666=CARTESIAN_POINT('Origin',(18.1457496550422,5.40110699657215,-0.999999999999995));
#8667=CARTESIAN_POINT('Origin',(19.3669593643482,-0.408193752494484,-1.));
#8668=CARTESIAN_POINT('Origin',(17.5759387331456,8.01789583575902,-1.));
#8669=CARTESIAN_POINT('',(18.4939069776058,1.47292913328138,-0.999999999999996));
#8670=CARTESIAN_POINT('Origin',(-4.20843915271973E-12,-0.121376657232797,
-0.999999999999996));
#8671=CARTESIAN_POINT('',(18.8965031381544,1.10271500310216,-0.999999999999996));
#8672=CARTESIAN_POINT('Origin',(18.8974104025717,1.50771398689259,-0.999999999999996));
#8673=CARTESIAN_POINT('Origin',(18.8841122085149,-4.42854337825293,-1.));
#8674=CARTESIAN_POINT('',(18.8965031381544,-1.34546831756689,-0.999999999999996));
#8675=CARTESIAN_POINT('Origin',(18.884112208515,4.18579006378818,-1.));
#8676=CARTESIAN_POINT('',(18.4939069776058,-1.71568244774611,-0.999999999999996));
#8677=CARTESIAN_POINT('Origin',(18.8974104025717,-1.75046730135732,-0.999999999999996));
#8678=CARTESIAN_POINT('Origin',(-1.14006026841196E-11,-0.121376657231028,
-0.999999999999996));
#8679=CARTESIAN_POINT('Origin',(17.5759387331454,-8.26064915022374,-0.999999999999996));
#8680=CARTESIAN_POINT('',(18.2290662400285,-5.24752289586362,-0.999999999999996));
#8681=CARTESIAN_POINT('Origin',(19.3669593643482,0.165440438029741,-1.00000000000001));
#8682=CARTESIAN_POINT('',(17.758295925753,-5.52594251059977,-0.999999999999996));
#8683=CARTESIAN_POINT('Origin',(18.1457496550421,-5.64386031103686,-0.999999999999996));
#8684=CARTESIAN_POINT('Origin',(-7.66747776381749E-12,-0.121376657229412,
-0.999999999999996));
#8685=CARTESIAN_POINT('Origin',(15.4996123964262,-11.7370296576882,-1.00000000000001));
#8686=CARTESIAN_POINT('',(16.7649316744485,-8.92554028555341,-0.999999999999996));
#8687=CARTESIAN_POINT('Origin',(19.0033774629777,-3.86744447109281,-1.));
#8688=CARTESIAN_POINT('',(16.2465621281866,-9.09999711167697,-0.999999999999996));
#8689=CARTESIAN_POINT('Origin',(16.6010325746197,-9.29589428522849,-0.999999999999996));
#8690=CARTESIAN_POINT('Origin',(-5.0636578263763E-12,-0.121376657229021,
-0.999999999999996));
#8691=CARTESIAN_POINT('Origin',(12.7458786225911,-14.7057503909454,-1.));
#8692=CARTESIAN_POINT('',(14.5680891476275,-12.2187734776212,-0.999999999999996));
#8693=CARTESIAN_POINT('Origin',(17.8092567781527,-7.73660824112183,-1.00000000000001));
#8694=CARTESIAN_POINT('',(14.0247756059639,-12.2816429146939,-0.999999999999996));
#8695=CARTESIAN_POINT('Origin',(14.330770710094,-12.5469578148567,-0.999999999999996));
#8696=CARTESIAN_POINT('Origin',(2.40519409944184E-12,-0.121376657234426,
-0.999999999999996));
#8697=CARTESIAN_POINT('Origin',(9.43508879143727,-17.0370640084498,-0.999999999999996));
#8698=CARTESIAN_POINT('',(11.7345512196075,-14.9832923788876,-0.999999999999996));
#8699=CARTESIAN_POINT('Origin',(15.836786113827,-11.2729498489996,-1.00000000000001));
#8700=CARTESIAN_POINT('',(11.1900390914206,-14.9318267308282,-0.999999999999996));
#8701=CARTESIAN_POINT('Origin',(11.4341853988697,-15.254963823343,-0.999999999999996));
#8702=CARTESIAN_POINT('Origin',(1.15619319673854E-12,-0.121376657233852,
-0.999999999999996));
#8703=CARTESIAN_POINT('Origin',(5.71194030551854,-18.6290809182323,-1.));
#8704=CARTESIAN_POINT('',(8.38815709466665,-17.0982742477336,-0.999999999999996));
#8705=CARTESIAN_POINT('Origin',(13.172171902996,-14.3219141972119,-1.));
#8706=CARTESIAN_POINT('',(7.86624417281716,-16.934722810322,-0.999999999999996));
#8707=CARTESIAN_POINT('Origin',(8.03787131840589,-17.3015594536621,-0.999999999999996));
#8708=CARTESIAN_POINT('Origin',(-4.28953747522165E-12,-0.121376657222038,
-0.999999999999996));
#8709=CARTESIAN_POINT('',(4.67516025384533,-18.4712842276818,-0.999999999999996));
#8710=CARTESIAN_POINT('Origin',(9.93187057291061,-16.7502469131877,-1.00000000000001));
#8711=CARTESIAN_POINT('',(4.1986566374342,-18.2027949835397,-0.999999999999996));
#8712=CARTESIAN_POINT('Origin',(4.29026369134186,-18.5972986561137,-0.999999999999996));
#8713=CARTESIAN_POINT('Origin',(2.61075883134509E-13,-0.121376657233687,
-0.999999999999996));
#8714=CARTESIAN_POINT('',(1.74510424621309,-21.650766132316,-0.999999999999996));
#8715=CARTESIAN_POINT('Origin',(-2.82976767018717E-13,-0.121376657227844,
-1.00000000000114));
#8716=CARTESIAN_POINT('',(0.757836476023318,-19.0423151941755,-0.999999999999996));
#8717=CARTESIAN_POINT('Origin',(6.25749884038654,-18.4518182048057,-1.));
#8718=CARTESIAN_POINT('',(0.347567659605753,-18.6806224116263,-0.999999999999996));
#8719=CARTESIAN_POINT('Origin',(0.355150953997144,-19.085551409904,-0.999999999999996));
#8720=CARTESIAN_POINT('',(-0.347567659605688,-18.6806224116263,-0.999999999999996));
#8721=CARTESIAN_POINT('Origin',(4.2148359455374E-14,-0.12137665722483,-0.999999999999996));
#8722=CARTESIAN_POINT('',(-0.757836476023246,-19.0423151941755,-0.999999999999996));
#8723=CARTESIAN_POINT('Origin',(-0.355150953997086,-19.085551409904,-0.999999999999996));
#8724=CARTESIAN_POINT('Origin',(-6.25749884038644,-18.4518182048057,-1.));
#8725=CARTESIAN_POINT('',(-3.19260839230403,-18.7864103538685,-0.999999999999996));
#8726=CARTESIAN_POINT('Origin',(2.30964438172655,-19.3522612415774,-1.));
#8727=CARTESIAN_POINT('',(-3.51871169276238,-18.3473217431041,-0.999999999999996));
#8728=CARTESIAN_POINT('Origin',(-3.59548358424083,-18.7449787267958,-0.999999999999996));
#8729=CARTESIAN_POINT('',(-4.19865663743438,-18.2027949835397,-0.999999999999996));
#8730=CARTESIAN_POINT('Origin',(1.19327291103755E-12,-0.121376657226644,
-0.999999999999996));
#8731=CARTESIAN_POINT('',(-4.6751602538455,-18.4712842276817,-0.999999999999996));
#8732=CARTESIAN_POINT('Origin',(-4.29026369134204,-18.5972986561136,-0.999999999999996));
#8733=CARTESIAN_POINT('Origin',(-9.93187057291073,-16.7502469131876,-1.));
#8734=CARTESIAN_POINT('',(-7.00352095405292,-17.7147539762497,-0.999999999999996));
#8735=CARTESIAN_POINT('Origin',(-1.73915261931825,-19.4122223419907,-1.));
#8736=CARTESIAN_POINT('',(-7.23120645950477,-17.2174598165414,-0.999999999999996));
#8737=CARTESIAN_POINT('Origin',(-7.38897823680306,-17.59046526729,-0.999999999999996));
#8738=CARTESIAN_POINT('',(-7.86624417281732,-16.9347228103219,-0.999999999999996));
#8739=CARTESIAN_POINT('Origin',(4.03409944338406E-12,-0.121376657223046,
-0.999999999999996));
#8740=CARTESIAN_POINT('',(-8.38815709466681,-17.0982742477335,-0.999999999999996));
#8741=CARTESIAN_POINT('Origin',(-8.03787131840607,-17.301559453662,-0.999999999999995));
#8742=CARTESIAN_POINT('Origin',(-13.1721719029961,-14.3219141972117,-0.999999999999996));
#8743=CARTESIAN_POINT('',(-10.5083460434876,-15.874182587399,-0.999999999999996));
#8744=CARTESIAN_POINT('Origin',(-5.7119403055187,-18.6290809182322,-0.999999999999996));
#8745=CARTESIAN_POINT('',(-10.6276628047884,-15.3404170198082,-0.999999999999996));
#8746=CARTESIAN_POINT('Origin',(-10.8595390841656,-15.6724688095371,-0.999999999999996));
#8747=CARTESIAN_POINT('',(-11.1900390914207,-14.931826730828,-0.999999999999996));
#8748=CARTESIAN_POINT('Origin',(6.0281640790194E-13,-0.121376657231363,
-0.999999999999996));
#8749=CARTESIAN_POINT('',(-11.7345512196077,-14.9832923788874,-0.999999999999996));
#8750=CARTESIAN_POINT('Origin',(-11.4341853988699,-15.2549638233429,-0.999999999999995));
#8751=CARTESIAN_POINT('Origin',(-15.8367861138271,-11.2729498489993,-1.));
#8752=CARTESIAN_POINT('',(1.49999999999993,5.62862334276781,-0.999999999999996));
#8753=CARTESIAN_POINT('',(-1.49999999999993,5.62862334276781,-0.999999999999996));
#8754=CARTESIAN_POINT('',(3.55704336920074E-14,5.62862334276781,-0.999999999999996));
#8755=CARTESIAN_POINT('',(-1.49999999999993,-0.121376657232177,-0.999999999999996));
#8756=CARTESIAN_POINT('',(1.49999999999993,-0.121376657232177,-0.999999999999996));
#8757=CARTESIAN_POINT('Origin',(3.55704336920074E-14,-0.121376657232177,
1.));
#8758=CARTESIAN_POINT('',(-13.5539059861829,-13.3451379890505,1.));
#8759=CARTESIAN_POINT('Origin',(-9.43508879143742,-17.0370640084497,1.00000000000001));
#8760=CARTESIAN_POINT('',(-11.7345512196077,-14.9832923788874,1.));
#8761=CARTESIAN_POINT('Origin',(-15.8367861138271,-11.2729498489993,1.00000000000001));
#8762=CARTESIAN_POINT('',(-11.1900390914207,-14.931826730828,1.));
#8763=CARTESIAN_POINT('Origin',(-11.4341853988699,-15.2549638233429,1.));
#8764=CARTESIAN_POINT('',(-10.6276628047884,-15.3404170198082,1.));
#8765=CARTESIAN_POINT('Origin',(6.0281640790194E-13,-0.121376657231363,
1.));
#8766=CARTESIAN_POINT('',(-10.5083460434876,-15.874182587399,1.));
#8767=CARTESIAN_POINT('Origin',(-10.8595390841656,-15.6724688095371,1.));
#8768=CARTESIAN_POINT('Origin',(-5.7119403055187,-18.6290809182322,1.00000000000001));
#8769=CARTESIAN_POINT('',(-8.38815709466681,-17.0982742477335,1.));
#8770=CARTESIAN_POINT('Origin',(-13.1721719029961,-14.3219141972117,1.));
#8771=CARTESIAN_POINT('',(-7.86624417281732,-16.9347228103219,1.));
#8772=CARTESIAN_POINT('Origin',(-8.03787131840606,-17.301559453662,1.));
#8773=CARTESIAN_POINT('',(-7.23120645950477,-17.2174598165414,1.));
#8774=CARTESIAN_POINT('Origin',(4.03409944338406E-12,-0.121376657223046,
1.));
#8775=CARTESIAN_POINT('',(-7.00352095405292,-17.7147539762497,1.));
#8776=CARTESIAN_POINT('Origin',(-7.38897823680306,-17.59046526729,1.));
#8777=CARTESIAN_POINT('Origin',(-1.73915261931826,-19.4122223419907,1.));
#8778=CARTESIAN_POINT('',(-4.6751602538455,-18.4712842276817,1.));
#8779=CARTESIAN_POINT('Origin',(-9.93187057291071,-16.7502469131876,1.00000000000001));
#8780=CARTESIAN_POINT('',(-4.19865663743438,-18.2027949835397,1.));
#8781=CARTESIAN_POINT('Origin',(-4.29026369134204,-18.5972986561136,1.));
#8782=CARTESIAN_POINT('',(-3.51871169276238,-18.3473217431041,1.));
#8783=CARTESIAN_POINT('Origin',(1.19327291103755E-12,-0.121376657226644,
1.));
#8784=CARTESIAN_POINT('',(-3.19260839230403,-18.7864103538685,1.));
#8785=CARTESIAN_POINT('Origin',(-3.59548358424083,-18.7449787267958,1.));
#8786=CARTESIAN_POINT('Origin',(2.30964438172659,-19.3522612415774,1.00000000000001));
#8787=CARTESIAN_POINT('',(-0.757836476023246,-19.0423151941755,1.));
#8788=CARTESIAN_POINT('Origin',(-6.25749884038647,-18.4518182048057,1.00000000000001));
#8789=CARTESIAN_POINT('',(-0.347567659605688,-18.6806224116263,1.));
#8790=CARTESIAN_POINT('Origin',(-0.355150953997085,-19.085551409904,1.));
#8791=CARTESIAN_POINT('',(0.347567659605753,-18.6806224116263,1.));
#8792=CARTESIAN_POINT('Origin',(4.2148359455374E-14,-0.12137665722483,1.));
#8793=CARTESIAN_POINT('',(0.757836476023318,-19.0423151941755,1.));
#8794=CARTESIAN_POINT('Origin',(0.355150953997144,-19.085551409904,1.));
#8795=CARTESIAN_POINT('',(1.74510424621308,-21.650766132316,1.));
#8796=CARTESIAN_POINT('Origin',(6.25749884038654,-18.4518182048057,1.));
#8797=CARTESIAN_POINT('Origin',(4.24356730310826E-13,-0.121376657236306,
1.00000000000115));
#8798=CARTESIAN_POINT('',(4.1986566374342,-18.2027949835397,1.));
#8799=CARTESIAN_POINT('Origin',(2.61075883134509E-13,-0.121376657233687,
1.));
#8800=CARTESIAN_POINT('',(4.67516025384533,-18.4712842276818,1.));
#8801=CARTESIAN_POINT('Origin',(4.29026369134186,-18.5972986561137,1.));
#8802=CARTESIAN_POINT('Origin',(9.93187057291057,-16.7502469131877,1.00000000000001));
#8803=CARTESIAN_POINT('',(7.86624417281716,-16.934722810322,1.));
#8804=CARTESIAN_POINT('Origin',(-4.28953747522165E-12,-0.121376657222038,
1.));
#8805=CARTESIAN_POINT('',(8.38815709466665,-17.0982742477336,1.));
#8806=CARTESIAN_POINT('Origin',(8.03787131840589,-17.3015594536621,1.));
#8807=CARTESIAN_POINT('Origin',(13.172171902996,-14.3219141972118,1.00000000000001));
#8808=CARTESIAN_POINT('Origin',(5.7119403055185,-18.6290809182323,1.00000000000001));
#8809=CARTESIAN_POINT('',(11.1900390914206,-14.9318267308282,1.));
#8810=CARTESIAN_POINT('Origin',(1.15619319673854E-12,-0.121376657233852,
1.));
#8811=CARTESIAN_POINT('',(11.7345512196075,-14.9832923788876,1.));
#8812=CARTESIAN_POINT('Origin',(11.4341853988697,-15.254963823343,1.));
#8813=CARTESIAN_POINT('Origin',(15.836786113827,-11.2729498489996,1.00000000000001));
#8814=CARTESIAN_POINT('Origin',(9.43508879143727,-17.0370640084498,1.));
#8815=CARTESIAN_POINT('',(14.0247756059639,-12.2816429146939,1.));
#8816=CARTESIAN_POINT('Origin',(2.40519409944184E-12,-0.121376657234426,
1.));
#8817=CARTESIAN_POINT('',(14.5680891476275,-12.2187734776212,1.));
#8818=CARTESIAN_POINT('Origin',(14.330770710094,-12.5469578148567,1.));
#8819=CARTESIAN_POINT('Origin',(17.8092567781528,-7.73660824112176,1.00000000000001));
#8820=CARTESIAN_POINT('Origin',(12.745878622591,-14.7057503909455,1.00000000000001));
#8821=CARTESIAN_POINT('',(16.2465621281866,-9.09999711167697,1.));
#8822=CARTESIAN_POINT('Origin',(-5.0636578263763E-12,-0.121376657229021,
1.));
#8823=CARTESIAN_POINT('',(16.7649316744485,-8.92554028555341,1.));
#8824=CARTESIAN_POINT('Origin',(16.6010325746197,-9.29589428522849,1.));
#8825=CARTESIAN_POINT('Origin',(19.0033774629777,-3.86744447109278,1.00000000000001));
#8826=CARTESIAN_POINT('Origin',(15.4996123964262,-11.7370296576882,1.00000000000001));
#8827=CARTESIAN_POINT('',(17.758295925753,-5.52594251059977,1.));
#8828=CARTESIAN_POINT('Origin',(-7.66747776381749E-12,-0.121376657229412,
1.));
#8829=CARTESIAN_POINT('',(18.2290662400285,-5.24752289586362,1.));
#8830=CARTESIAN_POINT('Origin',(18.1457496550421,-5.64386031103686,1.));
#8831=CARTESIAN_POINT('Origin',(19.3669593643482,0.16544043802976,1.00000000000001));
#8832=CARTESIAN_POINT('Origin',(17.5759387331454,-8.26064915022377,1.00000000000001));
#8833=CARTESIAN_POINT('',(18.4939069776058,-1.71568244774611,1.));
#8834=CARTESIAN_POINT('Origin',(-1.14006026841196E-11,-0.121376657231028,
1.));
#8835=CARTESIAN_POINT('',(18.8965031381544,-1.34546831756689,1.));
#8836=CARTESIAN_POINT('Origin',(18.8974104025717,-1.75046730135732,1.));
#8837=CARTESIAN_POINT('Origin',(18.884112208515,4.18579006378822,1.00000000000001));
#8838=CARTESIAN_POINT('',(18.8965031381544,1.10271500310216,1.));
#8839=CARTESIAN_POINT('Origin',(18.8841122085149,-4.42854337825293,1.00000000000001));
#8840=CARTESIAN_POINT('',(18.4939069776058,1.47292913328138,1.));
#8841=CARTESIAN_POINT('Origin',(18.8974104025717,1.50771398689259,1.));
#8842=CARTESIAN_POINT('Origin',(-4.20843915271973E-12,-0.121376657232797,
1.));
#8843=CARTESIAN_POINT('Origin',(17.5759387331456,8.01789583575901,1.00000000000001));
#8844=CARTESIAN_POINT('',(18.2290662400286,5.0047695813989,1.));
#8845=CARTESIAN_POINT('Origin',(19.3669593643482,-0.408193752494475,1.00000000000001));
#8846=CARTESIAN_POINT('',(17.7582959257531,5.28318919613505,1.));
#8847=CARTESIAN_POINT('Origin',(18.1457496550422,5.40110699657215,1.));
#8848=CARTESIAN_POINT('Origin',(-2.30544749957318E-12,-0.121376657233087,
1.));
#8849=CARTESIAN_POINT('Origin',(15.4996123964264,11.4942763432235,1.));
#8850=CARTESIAN_POINT('',(16.7649316744487,8.68278697108871,1.));
#8851=CARTESIAN_POINT('Origin',(19.0033774629777,3.62469115662802,1.00000000000001));
#8852=CARTESIAN_POINT('',(16.2465621281868,8.85724379721227,1.));
#8853=CARTESIAN_POINT('Origin',(16.6010325746199,9.05314097076379,1.));
#8854=CARTESIAN_POINT('Origin',(-2.16666962149503E-12,-0.121376657233593,
1.));
#8855=CARTESIAN_POINT('Origin',(12.7458786225913,14.4629970764809,1.00000000000001));
#8856=CARTESIAN_POINT('',(14.5680891476277,11.9760201631566,1.));
#8857=CARTESIAN_POINT('Origin',(17.8092567781529,7.49385492665713,1.00000000000001));
#8858=CARTESIAN_POINT('',(14.0247756059641,12.0388896002292,1.));
#8859=CARTESIAN_POINT('Origin',(14.3307707100943,12.304204500392,1.));
#8860=CARTESIAN_POINT('Origin',(-1.08160008727154E-12,-0.121376657233035,
1.));
#8861=CARTESIAN_POINT('Origin',(9.43508879143764,16.7943106939852,1.00000000000001));
#8862=CARTESIAN_POINT('',(11.7345512196078,14.740539064423,1.));
#8863=CARTESIAN_POINT('Origin',(15.8367861138273,11.0301965345349,1.00000000000001));
#8864=CARTESIAN_POINT('',(11.1900390914209,14.6890734163636,1.));
#8865=CARTESIAN_POINT('Origin',(11.4341853988701,15.0122105088784,1.));
#8866=CARTESIAN_POINT('Origin',(2.03656536079677E-12,-0.121376657229092,
1.));
#8867=CARTESIAN_POINT('Origin',(5.71194030551894,18.3863276037678,1.00000000000001));
#8868=CARTESIAN_POINT('',(8.38815709466699,16.8555209332691,1.));
#8869=CARTESIAN_POINT('Origin',(13.1721719029963,14.0791608827472,1.00000000000001));
#8870=CARTESIAN_POINT('',(7.8662441728175,16.6919694958575,1.));
#8871=CARTESIAN_POINT('Origin',(8.03787131840625,17.0588061391976,1.));
#8872=CARTESIAN_POINT('Origin',(-4.48686227061401E-12,-0.121376657241696,
1.));
#8873=CARTESIAN_POINT('',(4.6751602538457,18.2285309132174,1.));
#8874=CARTESIAN_POINT('Origin',(9.93187057291089,16.5074935987231,1.00000000000001));
#8875=CARTESIAN_POINT('',(4.19865663743457,17.9600416690753,1.));
#8876=CARTESIAN_POINT('Origin',(4.29026369134224,18.3545453416492,1.));
#8877=CARTESIAN_POINT('Origin',(-1.20715069884536E-12,-0.121376657237335,
1.));
#8878=CARTESIAN_POINT('',(0.757836476023318,18.7995618797112,1.));
#8879=CARTESIAN_POINT('Origin',(6.25749884038657,18.2090648903413,1.00000000000001));
#8880=CARTESIAN_POINT('',(0.347567659605759,18.4378690971619,1.));
#8881=CARTESIAN_POINT('Origin',(0.355150953997157,18.8427980954396,1.));
#8882=CARTESIAN_POINT('',(-0.347567659605682,18.4378690971619,1.));
#8883=CARTESIAN_POINT('Origin',(3.74591850593742E-14,-0.121376657224663,
1.));
#8884=CARTESIAN_POINT('',(-0.757836476023246,18.7995618797112,1.));
#8885=CARTESIAN_POINT('Origin',(-0.355150953997079,18.8427980954396,1.));
#8886=CARTESIAN_POINT('Origin',(-6.25749884038647,18.2090648903413,1.00000000000001));
#8887=CARTESIAN_POINT('',(-3.19260839230391,18.5436570394042,1.));
#8888=CARTESIAN_POINT('Origin',(2.30964438172673,19.109507927113,1.00000000000001));
#8889=CARTESIAN_POINT('',(-3.51871169276225,18.1045684286397,1.));
#8890=CARTESIAN_POINT('Origin',(-3.5954835842407,18.5022254123315,1.));
#8891=CARTESIAN_POINT('',(-4.19865663743425,17.9600416690753,1.));
#8892=CARTESIAN_POINT('Origin',(1.46844342241437E-12,-0.121376657238497,
1.));
#8893=CARTESIAN_POINT('',(-4.67516025384538,18.2285309132174,1.));
#8894=CARTESIAN_POINT('Origin',(-4.29026369134191,18.3545453416493,1.));
#8895=CARTESIAN_POINT('Origin',(-9.93187057291062,16.5074935987233,1.00000000000001));
#8896=CARTESIAN_POINT('',(-7.0035209540528,17.4720006617854,1.));
#8897=CARTESIAN_POINT('Origin',(-1.7391526193181,19.1694690275264,1.00000000000001));
#8898=CARTESIAN_POINT('',(-7.23120645950465,16.9747065020771,1.));
#8899=CARTESIAN_POINT('Origin',(-7.38897823680293,17.3477119528257,1.));
#8900=CARTESIAN_POINT('',(-7.8662441728172,16.6919694958576,1.));
#8901=CARTESIAN_POINT('Origin',(5.46524631106493E-12,-0.12137665724324,
1.));
#8902=CARTESIAN_POINT('',(-8.38815709466669,16.8555209332692,1.));
#8903=CARTESIAN_POINT('Origin',(-8.03787131840593,17.0588061391977,1.));
#8904=CARTESIAN_POINT('Origin',(-13.1721719029961,14.0791608827473,1.00000000000001));
#8905=CARTESIAN_POINT('',(-10.5083460434875,15.6314292729347,1.));
#8906=CARTESIAN_POINT('Origin',(-5.71194030551858,18.3863276037679,1.00000000000001));
#8907=CARTESIAN_POINT('',(-10.6276628047883,15.0976637053439,1.));
#8908=CARTESIAN_POINT('Origin',(-10.8595390841655,15.4297154950728,1.));
#8909=CARTESIAN_POINT('',(-11.1900390914206,14.6890734163638,1.));
#8910=CARTESIAN_POINT('Origin',(-9.26342336171615E-13,-0.121376657230733,
1.));
#8911=CARTESIAN_POINT('',(-11.7345512196076,14.7405390644231,1.));
#8912=CARTESIAN_POINT('Origin',(-11.4341853988698,15.0122105088786,1.));
#8913=CARTESIAN_POINT('Origin',(-15.8367861138271,11.030196534535,1.00000000000001));
#8914=CARTESIAN_POINT('',(-13.5539059861829,13.1023846745862,1.));
#8915=CARTESIAN_POINT('Origin',(-9.43508879143725,16.7943106939854,1.00000000000001));
#8916=CARTESIAN_POINT('',(-13.5596392883185,12.555475815708,1.));
#8917=CARTESIAN_POINT('Origin',(-13.8554859637,12.8320616878448,1.));
#8918=CARTESIAN_POINT('',(-14.0247756059639,12.0388896002294,1.));
#8919=CARTESIAN_POINT('Origin',(1.06442632485937E-11,-0.1213766572417,1.));
#8920=CARTESIAN_POINT('',(-14.5680891476275,11.9760201631568,1.));
#8921=CARTESIAN_POINT('Origin',(-14.330770710094,12.3042045003922,1.));
#8922=CARTESIAN_POINT('Origin',(-17.8092567781527,7.49385492665735,1.00000000000001));
#8923=CARTESIAN_POINT('',(-16.0070951984252,9.99539825139022,1.));
#8924=CARTESIAN_POINT('Origin',(-12.745878622591,14.4629970764811,1.00000000000001));
#8925=CARTESIAN_POINT('',(-15.8989944685809,9.45924864271742,1.));
#8926=CARTESIAN_POINT('Origin',(-16.2458816206226,9.66828046744359,1.));
#8927=CARTESIAN_POINT('',(-16.2465621281866,8.85724379721251,1.));
#8928=CARTESIAN_POINT('Origin',(3.8372083288607E-12,-0.121376657234332,
1.));
#8929=CARTESIAN_POINT('',(-16.7649316744485,8.68278697108894,1.));
#8930=CARTESIAN_POINT('Origin',(-16.6010325746197,9.05314097076402,1.));
#8931=CARTESIAN_POINT('Origin',(-19.0033774629776,3.6246911566283,1.));
#8932=CARTESIAN_POINT('',(-17.7606975399316,6.44626021901535,1.));
#8933=CARTESIAN_POINT('Origin',(-15.4996123964262,11.4942763432236,1.00000000000001));
#8934=CARTESIAN_POINT('',(-17.5434872987263,5.94430217117825,1.));
#8935=CARTESIAN_POINT('Origin',(-17.9262542943349,6.0766442547072,1.));
#8936=CARTESIAN_POINT('',(-17.7582959257529,5.2831891961353,1.));
#8937=CARTESIAN_POINT('Origin',(7.0082828429463E-13,-0.121376657232305,
1.));
#8938=CARTESIAN_POINT('',(-18.2290662400284,5.00476958139915,1.));
#8939=CARTESIAN_POINT('Origin',(-18.1457496550421,5.40110699657241,1.));
#8940=CARTESIAN_POINT('Origin',(-19.3669593643481,-0.408193752494226,1.00000000000001));
#8941=CARTESIAN_POINT('',(-18.7380721736606,2.61008494013019,1.));
#8942=CARTESIAN_POINT('Origin',(-17.5759387331454,8.01789583575926,1.00000000000001));
#8943=CARTESIAN_POINT('',(-18.4212455509255,2.16425642848123,1.));
#8944=CARTESIAN_POINT('Origin',(-18.8231636356729,2.21412478671497,1.));
#8945=CARTESIAN_POINT('',(-18.4939069776057,1.47292913328164,1.));
#8946=CARTESIAN_POINT('Origin',(-3.32199545649559E-12,-0.121376657231894,
1.));
#8947=CARTESIAN_POINT('',(-18.8965031381544,1.10271500310242,1.));
#8948=CARTESIAN_POINT('Origin',(-18.8974104025716,1.50771398689285,1.));
#8949=CARTESIAN_POINT('Origin',(-18.8841122085149,-4.42854337825269,1.00000000000001));
#8950=CARTESIAN_POINT('',(-18.8965031381544,-1.34546831756664,1.));
#8951=CARTESIAN_POINT('Origin',(-18.8841122085148,4.18579006378843,1.00000000000001));
#8952=CARTESIAN_POINT('',(-18.4939069776057,-1.71568244774586,1.));
#8953=CARTESIAN_POINT('Origin',(-18.8974104025717,-1.75046730135707,1.));
#8954=CARTESIAN_POINT('',(-18.4212455509255,-2.40700974294545,1.));
#8955=CARTESIAN_POINT('Origin',(3.52669282666085E-12,-0.121376657231728,
1.));
#8956=CARTESIAN_POINT('',(-18.7380721736606,-2.85283825459442,1.));
#8957=CARTESIAN_POINT('Origin',(-18.8231636356729,-2.45687810117919,1.));
#8958=CARTESIAN_POINT('Origin',(-17.5759387331454,-8.26064915022349,1.00000000000001));
#8959=CARTESIAN_POINT('',(-18.2290662400285,-5.24752289586338,1.));
#8960=CARTESIAN_POINT('Origin',(-19.3669593643481,0.16544043803,1.00000000000001));
#8961=CARTESIAN_POINT('',(-17.758295925753,-5.52594251059953,1.));
#8962=CARTESIAN_POINT('Origin',(-18.1457496550421,-5.64386031103663,1.));
#8963=CARTESIAN_POINT('',(-17.5434872987264,-6.18705548564248,1.));
#8964=CARTESIAN_POINT('Origin',(9.73179870022989E-13,-0.121376657231793,
1.));
#8965=CARTESIAN_POINT('',(-17.7606975399316,-6.68901353347958,1.));
#8966=CARTESIAN_POINT('Origin',(-17.926254294335,-6.31939756917143,1.));
#8967=CARTESIAN_POINT('Origin',(-15.4996123964263,-11.7370296576879,1.));
#8968=CARTESIAN_POINT('',(-16.7649316744485,-8.92554028555318,1.));
#8969=CARTESIAN_POINT('Origin',(-19.0033774629776,-3.86744447109251,1.00000000000001));
#8970=CARTESIAN_POINT('',(-16.2465621281866,-9.09999711167674,1.));
#8971=CARTESIAN_POINT('Origin',(-16.6010325746198,-9.29589428522826,1.));
#8972=CARTESIAN_POINT('',(-15.8989944685809,-9.70200195718166,1.));
#8973=CARTESIAN_POINT('Origin',(-2.48412401759879E-12,-0.121376657233779,
1.));
#8974=CARTESIAN_POINT('',(-16.0070951984253,-10.2381515658545,1.));
#8975=CARTESIAN_POINT('Origin',(-16.2458816206227,-9.91103378190783,1.));
#8976=CARTESIAN_POINT('Origin',(-12.7458786225912,-14.7057503909453,1.00000000000001));
#8977=CARTESIAN_POINT('',(-14.5680891476276,-12.218773477621,1.));
#8978=CARTESIAN_POINT('Origin',(-17.8092567781527,-7.73660824112161,1.));
#8979=CARTESIAN_POINT('',(-14.024775605964,-12.2816429146937,1.));
#8980=CARTESIAN_POINT('Origin',(-14.3307707100941,-12.5469578148565,1.));
#8981=CARTESIAN_POINT('',(-13.5596392883186,-12.7982291301722,1.));
#8982=CARTESIAN_POINT('Origin',(-8.74300631892311E-13,-0.121376657233123,
1.));
#8983=CARTESIAN_POINT('Origin',(-13.8554859637001,-13.0748150023091,1.));
#8984=CARTESIAN_POINT('',(-1.49999999999993,5.62862334276781,1.));
#8985=CARTESIAN_POINT('',(-1.49999999999993,5.62862334276781,1.));
#8986=CARTESIAN_POINT('',(1.49999999999993,5.62862334276781,1.));
#8987=CARTESIAN_POINT('',(-1.49999999999993,5.62862334276781,1.));
#8988=CARTESIAN_POINT('',(1.49999999999993,5.62862334276781,1.));
#8989=CARTESIAN_POINT('Origin',(3.64291929955129E-14,-0.121376657232174,
1.));
#8990=CARTESIAN_POINT('',(1.74510424621309,-21.650766132316,4.082419099807E-15));
#8991=CARTESIAN_POINT('Origin',(-6.25749884038648,-18.4518182048057,-0.999999999999996));
#8992=CARTESIAN_POINT('',(-0.757836476023246,-19.0423151941755,-0.999999999999996));
#8993=CARTESIAN_POINT('Origin',(6.25749884038655,-18.4518182048057,-0.999999999999996));
#8994=CARTESIAN_POINT('',(0.757836476023317,-19.0423151941755,-0.999999999999996));
#8995=CARTESIAN_POINT('Origin',(3.64291929955129E-14,-0.121376657232175,
-0.999999999999996));
#8996=CARTESIAN_POINT('',(-0.347567659605688,-18.6806224116263,-0.999999999999996));
#8997=CARTESIAN_POINT('',(0.347567659605753,-18.6806224116263,-0.999999999999996));
#8998=CARTESIAN_POINT('Origin',(-0.355150953997086,-19.085551409904,-0.999999999999996));
#8999=CARTESIAN_POINT('Origin',(0.355150953997151,-19.085551409904,-0.999999999999996));
#9000=CARTESIAN_POINT('Origin',(2.30964438172655,-19.3522612415774,-0.999999999999996));
#9001=CARTESIAN_POINT('',(-3.19260839230403,-18.7864103538685,-0.999999999999996));
#9002=CARTESIAN_POINT('Origin',(-9.93187057291073,-16.7502469131875,-0.999999999999996));
#9003=CARTESIAN_POINT('',(-4.6751602538455,-18.4712842276817,-0.999999999999996));
#9004=CARTESIAN_POINT('Origin',(-4.29026369134204,-18.5972986561136,-0.999999999999996));
#9005=CARTESIAN_POINT('',(-4.19865663743438,-18.2027949835397,-0.999999999999996));
#9006=CARTESIAN_POINT('Origin',(3.64291929955129E-14,-0.121376657232175,
-0.999999999999996));
#9007=CARTESIAN_POINT('',(-3.51871169276238,-18.3473217431041,-0.999999999999996));
#9008=CARTESIAN_POINT('Origin',(-3.59548358424083,-18.7449787267958,-0.999999999999996));
#9009=CARTESIAN_POINT('Origin',(15.4996123964264,11.4942763432235,-0.999999999999996));
#9010=CARTESIAN_POINT('Origin',(19.3669593643482,-0.408193752494492,-0.999999999999996));
#9011=CARTESIAN_POINT('',(18.2290662400286,5.0047695813989,-0.999999999999996));
#9012=CARTESIAN_POINT('Origin',(18.1457496550422,5.40110699657215,-0.999999999999996));
#9013=CARTESIAN_POINT('',(17.7582959257531,5.28318919613505,-0.999999999999996));
#9014=CARTESIAN_POINT('Origin',(3.64291929955129E-14,-0.121376657232175,
-0.999999999999996));
#9015=CARTESIAN_POINT('Origin',(12.7458786225913,14.4629970764809,-0.999999999999996));
#9016=CARTESIAN_POINT('Origin',(19.0033774629777,3.62469115662802,-0.999999999999996));
#9017=CARTESIAN_POINT('',(16.7649316744487,8.68278697108871,-0.999999999999996));
#9018=CARTESIAN_POINT('Origin',(16.6010325746199,9.05314097076379,-0.999999999999996));
#9019=CARTESIAN_POINT('',(16.2465621281868,8.85724379721227,-0.999999999999996));
#9020=CARTESIAN_POINT('Origin',(3.64291929955129E-14,-0.121376657232175,
-0.999999999999996));
#9021=CARTESIAN_POINT('Origin',(5.71194030551891,18.3863276037678,-0.999999999999996));
#9022=CARTESIAN_POINT('Origin',(15.8367861138273,11.0301965345348,-0.999999999999996));
#9023=CARTESIAN_POINT('',(11.7345512196078,14.740539064423,-0.999999999999996));
#9024=CARTESIAN_POINT('Origin',(11.4341853988701,15.0122105088784,-0.999999999999996));
#9025=CARTESIAN_POINT('',(11.1900390914209,14.6890734163636,-0.999999999999996));
#9026=CARTESIAN_POINT('Origin',(3.64291929955129E-14,-0.121376657232175,
-0.999999999999996));
#9027=CARTESIAN_POINT('Origin',(9.4350887914376,16.7943106939853,-0.999999999999996));
#9028=CARTESIAN_POINT('Origin',(17.8092567781529,7.49385492665712,-0.999999999999996));
#9029=CARTESIAN_POINT('',(14.5680891476277,11.9760201631566,-0.999999999999996));
#9030=CARTESIAN_POINT('Origin',(14.3307707100943,12.304204500392,-0.999999999999996));
#9031=CARTESIAN_POINT('',(14.0247756059641,12.0388896002292,-0.999999999999996));
#9032=CARTESIAN_POINT('Origin',(3.64291929955129E-14,-0.121376657232175,
-0.999999999999996));
#9033=CARTESIAN_POINT('Origin',(17.5759387331456,8.01789583575903,-0.999999999999996));
#9034=CARTESIAN_POINT('Origin',(18.8841122085149,-4.42854337825292,-0.999999999999996));
#9035=CARTESIAN_POINT('',(18.8965031381544,1.10271500310216,-0.999999999999996));
#9036=CARTESIAN_POINT('Origin',(18.8974104025717,1.50771398689258,-0.999999999999996));
#9037=CARTESIAN_POINT('',(18.4939069776058,1.47292913328138,-0.999999999999996));
#9038=CARTESIAN_POINT('Origin',(3.64291929955129E-14,-0.121376657232175,
-0.999999999999996));
#9039=CARTESIAN_POINT('Origin',(18.884112208515,4.18579006378819,-0.999999999999996));
#9040=CARTESIAN_POINT('',(18.8965031381544,-1.34546831756689,-0.999999999999996));
#9041=CARTESIAN_POINT('Origin',(17.5759387331454,-8.26064915022373,-0.999999999999996));
#9042=CARTESIAN_POINT('Origin',(3.64291929955129E-14,-0.121376657232175,
-0.999999999999996));
#9043=CARTESIAN_POINT('',(18.4939069776058,-1.71568244774611,-0.999999999999996));
#9044=CARTESIAN_POINT('Origin',(18.8974104025717,-1.75046730135732,-0.999999999999996));
#9045=CARTESIAN_POINT('Origin',(19.3669593643482,0.165440438029751,-0.999999999999996));
#9046=CARTESIAN_POINT('',(18.2290662400285,-5.24752289586362,-0.999999999999996));
#9047=CARTESIAN_POINT('Origin',(15.4996123964262,-11.7370296576881,-0.999999999999996));
#9048=CARTESIAN_POINT('Origin',(3.64291929955129E-14,-0.121376657232175,
-0.999999999999996));
#9049=CARTESIAN_POINT('',(17.758295925753,-5.52594251059977,-0.999999999999996));
#9050=CARTESIAN_POINT('Origin',(18.1457496550421,-5.64386031103687,-0.999999999999996));
#9051=CARTESIAN_POINT('Origin',(19.0033774629777,-3.86744447109277,-0.999999999999996));
#9052=CARTESIAN_POINT('',(16.7649316744485,-8.92554028555341,-0.999999999999996));
#9053=CARTESIAN_POINT('Origin',(12.745878622591,-14.7057503909455,-0.999999999999996));
#9054=CARTESIAN_POINT('Origin',(3.64291929955129E-14,-0.121376657232175,
-0.999999999999996));
#9055=CARTESIAN_POINT('',(16.2465621281866,-9.09999711167697,-0.999999999999996));
#9056=CARTESIAN_POINT('Origin',(16.6010325746197,-9.29589428522849,-0.999999999999996));
#9057=CARTESIAN_POINT('Origin',(15.836786113827,-11.2729498489995,-0.999999999999996));
#9058=CARTESIAN_POINT('',(11.7345512196075,-14.9832923788876,-0.999999999999996));
#9059=CARTESIAN_POINT('Origin',(5.71194030551853,-18.6290809182323,-0.999999999999996));
#9060=CARTESIAN_POINT('Origin',(3.64291929955129E-14,-0.121376657232175,
-0.999999999999996));
#9061=CARTESIAN_POINT('',(11.1900390914206,-14.9318267308282,-0.999999999999996));
#9062=CARTESIAN_POINT('Origin',(11.4341853988697,-15.254963823343,-0.999999999999996));
#9063=CARTESIAN_POINT('Origin',(17.8092567781527,-7.73660824112183,-0.999999999999996));
#9064=CARTESIAN_POINT('',(14.5680891476275,-12.2187734776212,-0.999999999999996));
#9065=CARTESIAN_POINT('Origin',(9.43508879143726,-17.0370640084498,-0.999999999999996));
#9066=CARTESIAN_POINT('Origin',(3.64291929955129E-14,-0.121376657232175,
-0.999999999999996));
#9067=CARTESIAN_POINT('',(14.0247756059639,-12.2816429146939,-0.999999999999996));
#9068=CARTESIAN_POINT('Origin',(14.330770710094,-12.5469578148567,-0.999999999999996));
#9069=CARTESIAN_POINT('Origin',(13.172171902996,-14.3219141972118,-0.999999999999996));
#9070=CARTESIAN_POINT('',(8.38815709466665,-17.0982742477336,-0.999999999999996));
#9071=CARTESIAN_POINT('Origin',(3.64291929955129E-14,-0.121376657232175,
-0.999999999999996));
#9072=CARTESIAN_POINT('',(7.86624417281716,-16.934722810322,-0.999999999999996));
#9073=CARTESIAN_POINT('Origin',(8.0378713184059,-17.3015594536621,-0.999999999999996));
#9074=CARTESIAN_POINT('Origin',(9.93187057291058,-16.7502469131877,-0.999999999999996));
#9075=CARTESIAN_POINT('',(4.67516025384533,-18.4712842276818,-0.999999999999996));
#9076=CARTESIAN_POINT('Origin',(3.64291929955129E-14,-0.121376657232175,
-0.999999999999996));
#9077=CARTESIAN_POINT('',(4.1986566374342,-18.2027949835397,-0.999999999999996));
#9078=CARTESIAN_POINT('Origin',(4.29026369134186,-18.5972986561137,-0.999999999999996));
#9079=CARTESIAN_POINT('Origin',(13.1721719029963,14.0791608827472,-0.999999999999996));
#9080=CARTESIAN_POINT('',(8.38815709466699,16.8555209332691,-0.999999999999996));
#9081=CARTESIAN_POINT('Origin',(8.03787131840625,17.0588061391976,-0.999999999999996));
#9082=CARTESIAN_POINT('',(7.8662441728175,16.6919694958575,-0.999999999999996));
#9083=CARTESIAN_POINT('Origin',(3.64291929955129E-14,-0.121376657232175,
-0.999999999999996));
#9084=CARTESIAN_POINT('Origin',(9.93187057291091,16.5074935987231,-0.999999999999996));
#9085=CARTESIAN_POINT('',(4.6751602538457,18.2285309132174,-0.999999999999996));
#9086=CARTESIAN_POINT('Origin',(4.29026369134223,18.3545453416492,-0.999999999999996));
#9087=CARTESIAN_POINT('',(4.19865663743457,17.9600416690753,-0.999999999999996));
#9088=CARTESIAN_POINT('Origin',(3.64291929955129E-14,-0.121376657232175,
-0.999999999999996));
#9089=CARTESIAN_POINT('Origin',(-6.25749884038648,18.2090648903413,-0.999999999999996));
#9090=CARTESIAN_POINT('',(-0.757836476023246,18.7995618797112,-0.999999999999996));
#9091=CARTESIAN_POINT('Origin',(6.25749884038655,18.2090648903413,-0.999999999999996));
#9092=CARTESIAN_POINT('',(0.757836476023318,18.7995618797112,-0.999999999999996));
#9093=CARTESIAN_POINT('Origin',(0.355150953997157,18.8427980954396,-0.999999999999996));
#9094=CARTESIAN_POINT('',(0.347567659605759,18.4378690971619,-0.999999999999996));
#9095=CARTESIAN_POINT('Origin',(3.64291929955129E-14,-0.121376657232175,
-0.999999999999996));
#9096=CARTESIAN_POINT('',(-0.347567659605682,18.4378690971619,-0.999999999999996));
#9097=CARTESIAN_POINT('Origin',(-0.355150953997079,18.8427980954396,-0.999999999999996));
#9098=CARTESIAN_POINT('Origin',(-9.93187057291061,16.5074935987233,-0.999999999999996));
#9099=CARTESIAN_POINT('',(-4.67516025384538,18.2285309132174,-0.999999999999996));
#9100=CARTESIAN_POINT('Origin',(2.30964438172668,19.109507927113,-0.999999999999996));
#9101=CARTESIAN_POINT('',(-3.19260839230391,18.5436570394042,-0.999999999999996));
#9102=CARTESIAN_POINT('Origin',(-3.5954835842407,18.5022254123315,-0.999999999999996));
#9103=CARTESIAN_POINT('',(-3.51871169276225,18.1045684286397,-0.999999999999996));
#9104=CARTESIAN_POINT('Origin',(3.64291929955129E-14,-0.121376657232175,
-0.999999999999996));
#9105=CARTESIAN_POINT('',(-4.19865663743425,17.9600416690753,-0.999999999999996));
#9106=CARTESIAN_POINT('Origin',(-4.29026369134191,18.3545453416493,-0.999999999999996));
#9107=CARTESIAN_POINT('Origin',(-17.8092567781527,7.49385492665736,-0.999999999999996));
#9108=CARTESIAN_POINT('',(-14.5680891476275,11.9760201631568,-0.999999999999996));
#9109=CARTESIAN_POINT('Origin',(-9.4350887914373,16.7943106939854,-0.999999999999996));
#9110=CARTESIAN_POINT('',(-13.5539059861829,13.1023846745862,-0.999999999999996));
#9111=CARTESIAN_POINT('Origin',(-13.8554859637,12.8320616878448,-0.999999999999996));
#9112=CARTESIAN_POINT('',(-13.5596392883185,12.555475815708,-0.999999999999996));
#9113=CARTESIAN_POINT('Origin',(3.64291929955129E-14,-0.121376657232175,
-0.999999999999996));
#9114=CARTESIAN_POINT('',(-14.0247756059639,12.0388896002294,-0.999999999999996));
#9115=CARTESIAN_POINT('Origin',(-14.330770710094,12.3042045003922,-0.999999999999996));
#9116=CARTESIAN_POINT('Origin',(-19.0033774629776,3.62469115662829,-0.999999999999996));
#9117=CARTESIAN_POINT('',(-16.7649316744485,8.68278697108894,-0.999999999999996));
#9118=CARTESIAN_POINT('Origin',(-12.7458786225911,14.462997076481,-0.999999999999996));
#9119=CARTESIAN_POINT('',(-16.0070951984252,9.99539825139022,-0.999999999999996));
#9120=CARTESIAN_POINT('Origin',(-16.2458816206226,9.66828046744359,-0.999999999999996));
#9121=CARTESIAN_POINT('',(-15.8989944685809,9.45924864271742,-0.999999999999996));
#9122=CARTESIAN_POINT('Origin',(3.64291929955129E-14,-0.121376657232175,
-0.999999999999996));
#9123=CARTESIAN_POINT('',(-16.2465621281866,8.85724379721251,-0.999999999999996));
#9124=CARTESIAN_POINT('Origin',(-16.6010325746197,9.05314097076402,-0.999999999999996));
#9125=CARTESIAN_POINT('Origin',(-15.8367861138271,11.0301965345351,-0.999999999999996));
#9126=CARTESIAN_POINT('',(-11.7345512196076,14.7405390644231,-0.999999999999996));
#9127=CARTESIAN_POINT('Origin',(-5.71194030551859,18.3863276037679,-0.999999999999996));
#9128=CARTESIAN_POINT('',(-10.5083460434875,15.6314292729347,-0.999999999999996));
#9129=CARTESIAN_POINT('Origin',(-10.8595390841655,15.4297154950728,-0.999999999999996));
#9130=CARTESIAN_POINT('',(-10.6276628047883,15.0976637053439,-0.999999999999996));
#9131=CARTESIAN_POINT('Origin',(3.64291929955129E-14,-0.121376657232175,
-0.999999999999996));
#9132=CARTESIAN_POINT('',(-11.1900390914206,14.6890734163638,-0.999999999999996));
#9133=CARTESIAN_POINT('Origin',(-11.4341853988698,15.0122105088786,-0.999999999999996));
#9134=CARTESIAN_POINT('Origin',(-13.1721719029961,14.0791608827474,-0.999999999999996));
#9135=CARTESIAN_POINT('',(-8.38815709466669,16.8555209332692,-0.999999999999996));
#9136=CARTESIAN_POINT('Origin',(-1.73915261931814,19.1694690275264,-0.999999999999996));
#9137=CARTESIAN_POINT('',(-7.0035209540528,17.4720006617854,-0.999999999999996));
#9138=CARTESIAN_POINT('Origin',(-7.38897823680293,17.3477119528256,-0.999999999999996));
#9139=CARTESIAN_POINT('',(-7.23120645950465,16.9747065020771,-0.999999999999996));
#9140=CARTESIAN_POINT('Origin',(3.64291929955129E-14,-0.121376657232175,
-0.999999999999996));
#9141=CARTESIAN_POINT('',(-7.8662441728172,16.6919694958576,-0.999999999999996));
#9142=CARTESIAN_POINT('Origin',(-8.03787131840594,17.0588061391977,-0.999999999999996));
#9143=CARTESIAN_POINT('Origin',(-19.3669593643481,-0.408193752494226,-0.999999999999996));
#9144=CARTESIAN_POINT('',(-18.2290662400284,5.00476958139915,-0.999999999999996));
#9145=CARTESIAN_POINT('Origin',(-15.4996123964262,11.4942763432237,-0.999999999999996));
#9146=CARTESIAN_POINT('',(-17.7606975399316,6.44626021901535,-0.999999999999996));
#9147=CARTESIAN_POINT('Origin',(-17.9262542943349,6.0766442547072,-0.999999999999996));
#9148=CARTESIAN_POINT('',(-17.5434872987263,5.94430217117825,-0.999999999999996));
#9149=CARTESIAN_POINT('Origin',(3.64291929955129E-14,-0.121376657232175,
-0.999999999999996));
#9150=CARTESIAN_POINT('',(-17.7582959257529,5.2831891961353,-0.999999999999996));
#9151=CARTESIAN_POINT('Origin',(-18.1457496550421,5.40110699657241,-0.999999999999996));
#9152=CARTESIAN_POINT('Origin',(-18.8841122085149,-4.42854337825267,-0.999999999999996));
#9153=CARTESIAN_POINT('',(-18.8965031381544,1.10271500310242,-0.999999999999996));
#9154=CARTESIAN_POINT('Origin',(-17.5759387331454,8.01789583575926,-0.999999999999996));
#9155=CARTESIAN_POINT('',(-18.7380721736606,2.61008494013019,-0.999999999999996));
#9156=CARTESIAN_POINT('Origin',(-18.8231636356729,2.21412478671498,-0.999999999999996));
#9157=CARTESIAN_POINT('',(-18.4212455509255,2.16425642848123,-0.999999999999996));
#9158=CARTESIAN_POINT('Origin',(3.64291929955129E-14,-0.121376657232175,
-0.999999999999996));
#9159=CARTESIAN_POINT('',(-18.4939069776057,1.47292913328164,-0.999999999999996));
#9160=CARTESIAN_POINT('Origin',(-18.8974104025716,1.50771398689285,-0.999999999999996));
#9161=CARTESIAN_POINT('Origin',(-17.5759387331454,-8.2606491502235,-0.999999999999996));
#9162=CARTESIAN_POINT('',(-18.7380721736606,-2.85283825459442,-0.999999999999996));
#9163=CARTESIAN_POINT('Origin',(-18.8841122085148,4.18579006378844,-0.999999999999996));
#9164=CARTESIAN_POINT('',(-18.8965031381544,-1.34546831756664,-0.999999999999996));
#9165=CARTESIAN_POINT('Origin',(-18.8974104025717,-1.75046730135707,-0.999999999999996));
#9166=CARTESIAN_POINT('',(-18.4939069776057,-1.71568244774586,-0.999999999999996));
#9167=CARTESIAN_POINT('Origin',(3.64291929955129E-14,-0.121376657232175,
-0.999999999999996));
#9168=CARTESIAN_POINT('',(-18.4212455509255,-2.40700974294545,-0.999999999999996));
#9169=CARTESIAN_POINT('Origin',(-18.8231636356729,-2.4568781011792,-0.999999999999996));
#9170=CARTESIAN_POINT('Origin',(-15.4996123964263,-11.7370296576879,-0.999999999999996));
#9171=CARTESIAN_POINT('',(-17.7606975399316,-6.68901353347958,-0.999999999999996));
#9172=CARTESIAN_POINT('Origin',(-19.3669593643481,0.165440438030005,-0.999999999999996));
#9173=CARTESIAN_POINT('',(-18.2290662400285,-5.24752289586338,-0.999999999999996));
#9174=CARTESIAN_POINT('Origin',(-18.1457496550421,-5.64386031103663,-0.999999999999996));
#9175=CARTESIAN_POINT('',(-17.758295925753,-5.52594251059953,-0.999999999999996));
#9176=CARTESIAN_POINT('Origin',(3.64291929955129E-14,-0.121376657232175,
-0.999999999999996));
#9177=CARTESIAN_POINT('',(-17.5434872987264,-6.18705548564248,-0.999999999999996));
#9178=CARTESIAN_POINT('Origin',(-17.926254294335,-6.31939756917143,-0.999999999999996));
#9179=CARTESIAN_POINT('Origin',(-1.73915261931827,-19.4122223419907,-0.999999999999996));
#9180=CARTESIAN_POINT('',(-7.00352095405292,-17.7147539762497,-0.999999999999996));
#9181=CARTESIAN_POINT('Origin',(-13.1721719029961,-14.3219141972116,-0.999999999999996));
#9182=CARTESIAN_POINT('',(-8.38815709466681,-17.0982742477335,-0.999999999999996));
#9183=CARTESIAN_POINT('Origin',(-8.03787131840606,-17.301559453662,-0.999999999999996));
#9184=CARTESIAN_POINT('',(-7.86624417281732,-16.9347228103219,-0.999999999999996));
#9185=CARTESIAN_POINT('Origin',(3.64291929955129E-14,-0.121376657232175,
-0.999999999999996));
#9186=CARTESIAN_POINT('',(-7.23120645950477,-17.2174598165414,-0.999999999999996));
#9187=CARTESIAN_POINT('Origin',(-7.38897823680305,-17.5904652672899,-0.999999999999996));
#9188=CARTESIAN_POINT('Origin',(-5.71194030551871,-18.6290809182322,-0.999999999999996));
#9189=CARTESIAN_POINT('',(-10.5083460434876,-15.874182587399,-0.999999999999996));
#9190=CARTESIAN_POINT('Origin',(-15.8367861138271,-11.2729498489993,-0.999999999999996));
#9191=CARTESIAN_POINT('',(-11.7345512196077,-14.9832923788874,-0.999999999999996));
#9192=CARTESIAN_POINT('Origin',(-11.4341853988699,-15.2549638233429,-0.999999999999996));
#9193=CARTESIAN_POINT('',(-11.1900390914207,-14.931826730828,-0.999999999999996));
#9194=CARTESIAN_POINT('Origin',(3.64291929955129E-14,-0.121376657232175,
-0.999999999999996));
#9195=CARTESIAN_POINT('',(-10.6276628047884,-15.3404170198082,-0.999999999999996));
#9196=CARTESIAN_POINT('Origin',(-10.8595390841656,-15.6724688095371,-0.999999999999996));
#9197=CARTESIAN_POINT('Origin',(-12.7458786225912,-14.7057503909453,-0.999999999999996));
#9198=CARTESIAN_POINT('',(-16.0070951984253,-10.2381515658545,-0.999999999999996));
#9199=CARTESIAN_POINT('Origin',(-19.0033774629776,-3.86744447109251,-0.999999999999996));
#9200=CARTESIAN_POINT('',(-16.7649316744485,-8.92554028555318,-0.999999999999996));
#9201=CARTESIAN_POINT('Origin',(-16.6010325746198,-9.29589428522826,-0.999999999999996));
#9202=CARTESIAN_POINT('',(-16.2465621281866,-9.09999711167674,-0.999999999999996));
#9203=CARTESIAN_POINT('Origin',(3.64291929955129E-14,-0.121376657232175,
-0.999999999999996));
#9204=CARTESIAN_POINT('',(-15.8989944685809,-9.70200195718166,-0.999999999999996));
#9205=CARTESIAN_POINT('Origin',(-16.2458816206227,-9.91103378190782,-0.999999999999996));
#9206=CARTESIAN_POINT('Origin',(-9.43508879143742,-17.0370640084497,-0.999999999999996));
#9207=CARTESIAN_POINT('',(-13.5539059861829,-13.3451379890505,-0.999999999999996));
#9208=CARTESIAN_POINT('Origin',(-17.8092567781528,-7.73660824112159,-0.999999999999996));
#9209=CARTESIAN_POINT('',(-14.5680891476276,-12.218773477621,-0.999999999999996));
#9210=CARTESIAN_POINT('Origin',(-14.3307707100941,-12.5469578148565,-0.999999999999996));
#9211=CARTESIAN_POINT('',(-14.024775605964,-12.2816429146937,-0.999999999999996));
#9212=CARTESIAN_POINT('Origin',(3.64291929955129E-14,-0.121376657232175,
-0.999999999999996));
#9213=CARTESIAN_POINT('',(-13.5596392883186,-12.7982291301722,-0.999999999999996));
#9214=CARTESIAN_POINT('Origin',(-13.8554859637001,-13.0748150023091,-0.999999999999996));
#9215=CARTESIAN_POINT('Origin',(-1.49999999999993,5.62862334276781,-4.));
#9216=CARTESIAN_POINT('',(1.49999999999993,5.62862334276781,-4.));
#9217=CARTESIAN_POINT('',(-1.49999999999993,5.62862334276781,-4.));
#9218=CARTESIAN_POINT('Origin',(-1.49999999999993,5.62862334276781,-4.));
#9219=CARTESIAN_POINT('Origin',(1.49999999999993,5.62862334276781,-4.));
#9220=CARTESIAN_POINT('',(0.,0.,0.));
#9221=CARTESIAN_POINT('Origin',(-3.25,0.,0.));
#9222=CARTESIAN_POINT('',(3.25,-4.163799117101E-16,-3.4));
#9223=CARTESIAN_POINT('Origin',(3.25,0.,0.));
#9224=CARTESIAN_POINT('',(-3.25,-4.163799117101E-16,-3.4));
#9225=CARTESIAN_POINT('',(-3.25,-4.163799117101E-16,-3.4));
#9226=CARTESIAN_POINT('Origin',(-3.25,0.,0.));
#9227=CARTESIAN_POINT('Origin',(3.25,0.,0.));
#9228=CARTESIAN_POINT('',(3.25,-3.25,5.62916512459885));
#9229=CARTESIAN_POINT('',(3.25,3.25,5.62916512459885));
#9230=CARTESIAN_POINT('Origin',(3.25,0.,0.));
#9231=CARTESIAN_POINT('',(2.66944341639924,1.02340605167262E-15,7.50555349946514));
#9232=CARTESIAN_POINT('Ctrl Pts',(2.66944341639009,-2.742976229949E-11,
7.50555349948097));
#9233=CARTESIAN_POINT('Ctrl Pts',(3.25,1.74166975079127,6.50000000000637));
#9234=CARTESIAN_POINT('Ctrl Pts',(3.25,3.24999999999999,5.62916512459886));
#9235=CARTESIAN_POINT('Ctrl Pts',(3.25,-3.25000000000001,5.62916512459885));
#9236=CARTESIAN_POINT('Ctrl Pts',(3.25,-1.74166975079127,6.50000000000637));
#9237=CARTESIAN_POINT('Ctrl Pts',(2.66944341639009,2.74484283507316E-11,
7.50555349948099));
#9238=CARTESIAN_POINT('Origin',(-3.25,0.,0.));
#9239=CARTESIAN_POINT('',(-3.25,3.25,5.62916512459885));
#9240=CARTESIAN_POINT('',(-3.25,-3.25,5.62916512459885));
#9241=CARTESIAN_POINT('Origin',(-3.25,0.,0.));
#9242=CARTESIAN_POINT('',(-2.66944341639924,8.87400251789783E-16,7.50555349946514));
#9243=CARTESIAN_POINT('Ctrl Pts',(-3.25,-3.25,5.62916512459885));
#9244=CARTESIAN_POINT('Ctrl Pts',(-3.25,-1.74166975079126,6.50000000000637));
#9245=CARTESIAN_POINT('Ctrl Pts',(-2.66944341639009,2.74493855841286E-11,
7.50555349948098));
#9246=CARTESIAN_POINT('Ctrl Pts',(-2.66944341639009,-2.742976229949E-11,
7.50555349948097));
#9247=CARTESIAN_POINT('Ctrl Pts',(-3.25,1.74166975079127,6.50000000000637));
#9248=CARTESIAN_POINT('Ctrl Pts',(-3.25,3.24999999999999,5.62916512459886));
#9249=CARTESIAN_POINT('Origin',(3.25,6.5,3.75277674973257));
#9250=CARTESIAN_POINT('',(3.25,8.57827996624955E-16,7.50555349946514));
#9251=CARTESIAN_POINT('',(2.66944341639923,6.5,3.75277674973257));
#9252=CARTESIAN_POINT('Ctrl Pts',(3.25,3.24999999999999,5.62916512459886));
#9253=CARTESIAN_POINT('Ctrl Pts',(3.25,4.75833024920873,4.75833024919134));
#9254=CARTESIAN_POINT('Ctrl Pts',(2.66944341639009,6.50000000002745,3.75277674971672));
#9255=CARTESIAN_POINT('',(-2.66944341639923,6.5,3.75277674973257));
#9256=CARTESIAN_POINT('',(3.25,6.5,3.75277674973257));
#9257=CARTESIAN_POINT('Ctrl Pts',(-3.25,3.25,5.62916512459885));
#9258=CARTESIAN_POINT('Ctrl Pts',(-3.25,4.75833024920873,4.75833024919133));
#9259=CARTESIAN_POINT('Ctrl Pts',(-2.66944341639009,6.50000000002744,3.75277674971672));
#9260=CARTESIAN_POINT('Origin',(3.25,8.57827996624955E-16,7.50555349946514));
#9261=CARTESIAN_POINT('',(2.66944341639924,-6.5,3.75277674973257));
#9262=CARTESIAN_POINT('',(-2.66944341639924,-6.5,3.75277674973257));
#9263=CARTESIAN_POINT('',(3.25,-6.5,3.75277674973257));
#9264=CARTESIAN_POINT('Ctrl Pts',(2.66944341639009,-6.50000000002745,3.75277674971672));
#9265=CARTESIAN_POINT('Ctrl Pts',(3.25,-4.75833024920874,4.75833024919133));
#9266=CARTESIAN_POINT('Ctrl Pts',(3.25,-3.25,5.62916512459885));
#9267=CARTESIAN_POINT('Ctrl Pts',(-2.66944341639009,-6.50000000002744,3.75277674971673));
#9268=CARTESIAN_POINT('Ctrl Pts',(-3.25,-4.75833024920873,4.75833024919134));
#9269=CARTESIAN_POINT('Ctrl Pts',(-3.25,-3.25,5.62916512459885));
#9270=CARTESIAN_POINT('Origin',(3.25,-6.5,3.75277674973257));
#9271=CARTESIAN_POINT('',(2.66944341639924,-6.5,-3.75277674973257));
#9272=CARTESIAN_POINT('',(-2.66944341639924,-6.5,-3.75277674973257));
#9273=CARTESIAN_POINT('',(3.25,-6.5,-3.75277674973257));
#9274=CARTESIAN_POINT('',(3.25,-6.5,3.00462919747432E-15));
#9275=CARTESIAN_POINT('Ctrl Pts',(2.66944341639009,-6.5,-3.75277674976425));
#9276=CARTESIAN_POINT('Ctrl Pts',(3.25,-6.5,-1.74166975081502));
#9277=CARTESIAN_POINT('Ctrl Pts',(3.25,-6.5,1.55488747964449E-14));
#9278=CARTESIAN_POINT('Ctrl Pts',(3.25,-6.5,1.55488747964449E-14));
#9279=CARTESIAN_POINT('Ctrl Pts',(3.25,-6.5,1.74166975081504));
#9280=CARTESIAN_POINT('Ctrl Pts',(2.66944341639009,-6.5,3.75277674976426));
#9281=CARTESIAN_POINT('',(-3.25,-6.5,3.00462919747432E-15));
#9282=CARTESIAN_POINT('Ctrl Pts',(-3.25,-6.5,8.88507131225421E-15));
#9283=CARTESIAN_POINT('Ctrl Pts',(-3.25,-6.5,1.74166975081504));
#9284=CARTESIAN_POINT('Ctrl Pts',(-2.66944341639009,-6.5,3.75277674976425));
#9285=CARTESIAN_POINT('Ctrl Pts',(-2.66944341639009,-6.5,-3.75277674976426));
#9286=CARTESIAN_POINT('Ctrl Pts',(-3.25,-6.5,-1.74166975081503));
#9287=CARTESIAN_POINT('Ctrl Pts',(-3.25,-6.5,8.88507131225421E-15));
#9288=CARTESIAN_POINT('Origin',(3.25,-6.5,-3.75277674973257));
#9289=CARTESIAN_POINT('',(2.66944341639924,1.85174857192461E-15,-7.50555349946513));
#9290=CARTESIAN_POINT('',(-2.66944341639924,1.85174857192461E-15,-7.50555349946513));
#9291=CARTESIAN_POINT('',(3.25,1.78461907357084E-15,-7.50555349946513));
#9292=CARTESIAN_POINT('',(3.25,-3.25,-5.62916512459885));
#9293=CARTESIAN_POINT('Ctrl Pts',(2.66944341639009,2.74386167084123E-11,
-7.50555349948098));
#9294=CARTESIAN_POINT('Ctrl Pts',(3.25,-1.74166975079127,-6.50000000000637));
#9295=CARTESIAN_POINT('Ctrl Pts',(3.25,-3.24999999999999,-5.62916512459886));
#9296=CARTESIAN_POINT('Ctrl Pts',(3.25,-3.24999999999999,-5.62916512459886));
#9297=CARTESIAN_POINT('Ctrl Pts',(3.25,-4.75833024920873,-4.75833024919134));
#9298=CARTESIAN_POINT('Ctrl Pts',(2.66944341639009,-6.50000000002745,-3.75277674971673));
#9299=CARTESIAN_POINT('',(-3.25,-3.25,-5.62916512459885));
#9300=CARTESIAN_POINT('Ctrl Pts',(-3.25,-3.25,-5.62916512459885));
#9301=CARTESIAN_POINT('Ctrl Pts',(-3.25,-4.75833024920873,-4.75833024919133));
#9302=CARTESIAN_POINT('Ctrl Pts',(-2.66944341639009,-6.50000000002744,-3.75277674971672));
#9303=CARTESIAN_POINT('Ctrl Pts',(-2.66944341639009,2.74465138839376E-11,
-7.50555349948098));
#9304=CARTESIAN_POINT('Ctrl Pts',(-3.25,-1.74166975079127,-6.50000000000637));
#9305=CARTESIAN_POINT('Ctrl Pts',(-3.25,-3.25,-5.62916512459885));
#9306=CARTESIAN_POINT('Origin',(3.25,1.78461907357084E-15,-7.50555349946513));
#9307=CARTESIAN_POINT('',(2.66944341639924,6.5,-3.75277674973257));
#9308=CARTESIAN_POINT('',(-2.66944341639924,6.5,-3.75277674973258));
#9309=CARTESIAN_POINT('',(3.25,6.5,-3.75277674973257));
#9310=CARTESIAN_POINT('',(3.25,3.25,-5.62916512459885));
#9311=CARTESIAN_POINT('Ctrl Pts',(2.66944341639009,6.50000000002744,-3.75277674971672));
#9312=CARTESIAN_POINT('Ctrl Pts',(3.25,4.75833024920874,-4.75833024919133));
#9313=CARTESIAN_POINT('Ctrl Pts',(3.25,3.25000000000001,-5.62916512459884));
#9314=CARTESIAN_POINT('Ctrl Pts',(3.25,3.25000000000001,-5.62916512459884));
#9315=CARTESIAN_POINT('Ctrl Pts',(3.25,1.74166975079128,-6.50000000000636));
#9316=CARTESIAN_POINT('Ctrl Pts',(2.66944341639009,-2.74398132501586E-11,
-7.50555349948098));
#9317=CARTESIAN_POINT('',(-3.25,3.25,-5.62916512459885));
#9318=CARTESIAN_POINT('Ctrl Pts',(-3.25,3.24999999999999,-5.62916512459886));
#9319=CARTESIAN_POINT('Ctrl Pts',(-3.25,1.74166975079126,-6.50000000000637));
#9320=CARTESIAN_POINT('Ctrl Pts',(-2.66944341639009,-2.74465138839376E-11,
-7.50555349948098));
#9321=CARTESIAN_POINT('Ctrl Pts',(-2.66944341639009,6.50000000002743,-3.75277674971672));
#9322=CARTESIAN_POINT('Ctrl Pts',(-3.25,4.75833024920872,-4.75833024919134));
#9323=CARTESIAN_POINT('Ctrl Pts',(-3.25,3.24999999999999,-5.62916512459886));
#9324=CARTESIAN_POINT('Origin',(3.25,6.5,-3.75277674973257));
#9325=CARTESIAN_POINT('',(3.25,6.5,-2.25347189810574E-15));
#9326=CARTESIAN_POINT('Ctrl Pts',(2.66944341639009,6.5,3.75277674976426));
#9327=CARTESIAN_POINT('Ctrl Pts',(3.25,6.5,1.74166975081503));
#9328=CARTESIAN_POINT('Ctrl Pts',(3.25,6.5,-7.10805704980337E-15));
#9329=CARTESIAN_POINT('Ctrl Pts',(3.25,6.5,-7.10805704980337E-15));
#9330=CARTESIAN_POINT('Ctrl Pts',(3.25,6.5,-1.74166975081504));
#9331=CARTESIAN_POINT('Ctrl Pts',(2.66944341639009,6.5,-3.75277674976425));
#9332=CARTESIAN_POINT('',(-3.25,6.5,-2.25347189810574E-15));
#9333=CARTESIAN_POINT('Ctrl Pts',(-3.25,6.5,-2.66552139367626E-15));
#9334=CARTESIAN_POINT('Ctrl Pts',(-3.25,6.5,-1.74166975081505));
#9335=CARTESIAN_POINT('Ctrl Pts',(-2.66944341639008,6.5,-3.75277674976428));
#9336=CARTESIAN_POINT('Ctrl Pts',(-2.66944341639009,6.5,3.75277674976426));
#9337=CARTESIAN_POINT('Ctrl Pts',(-3.25,6.5,1.74166975081503));
#9338=CARTESIAN_POINT('Ctrl Pts',(-3.25,6.5,-2.66552139367626E-15));
#9339=CARTESIAN_POINT('Origin',(-3.25,0.,0.));
#9340=CARTESIAN_POINT('Origin',(-3.25,0.,0.));
#9341=CARTESIAN_POINT('Origin',(-3.25,0.,0.));
#9342=CARTESIAN_POINT('Origin',(-3.25,0.,0.));
#9343=CARTESIAN_POINT('Origin',(-3.25,0.,0.));
#9344=CARTESIAN_POINT('Origin',(-3.25,0.,0.));
#9345=CARTESIAN_POINT('Origin',(-3.25,0.,0.));
#9346=CARTESIAN_POINT('Origin',(-3.25,0.,0.));
#9347=CARTESIAN_POINT('Origin',(-3.25,0.,0.));
#9348=CARTESIAN_POINT('Origin',(-3.25,0.,0.));
#9349=CARTESIAN_POINT('Origin',(-3.25,0.,0.));
#9350=CARTESIAN_POINT('Origin',(3.25,0.,0.));
#9351=CARTESIAN_POINT('Origin',(3.25,0.,0.));
#9352=CARTESIAN_POINT('Origin',(3.25,0.,0.));
#9353=CARTESIAN_POINT('Origin',(3.25,0.,0.));
#9354=CARTESIAN_POINT('Origin',(3.25,0.,0.));
#9355=CARTESIAN_POINT('Origin',(3.25,0.,0.));
#9356=CARTESIAN_POINT('Origin',(3.25,0.,0.));
#9357=CARTESIAN_POINT('Origin',(3.25,0.,0.));
#9358=CARTESIAN_POINT('Origin',(3.25,0.,0.));
#9359=CARTESIAN_POINT('Origin',(3.25,0.,0.));
#9360=CARTESIAN_POINT('Origin',(3.25,0.,0.));
#9361=CARTESIAN_POINT('',(0.,0.,0.));
#9362=CARTESIAN_POINT('Origin',(0.,0.,2.));
#9363=CARTESIAN_POINT('',(8.,-9.79717439317883E-16,2.));
#9364=CARTESIAN_POINT('Origin',(0.,0.,2.));
#9365=CARTESIAN_POINT('',(8.,-9.79717439317883E-16,0.));
#9366=CARTESIAN_POINT('',(8.,-9.79717439317883E-16,2.));
#9367=CARTESIAN_POINT('Origin',(0.,0.,0.));
#9368=CARTESIAN_POINT('Origin',(0.,0.,4.));
#9369=CARTESIAN_POINT('',(25.,-3.06161699786838E-15,0.));
#9370=CARTESIAN_POINT('Origin',(0.,0.,0.));
#9371=CARTESIAN_POINT('',(25.,-3.06161699786838E-15,4.));
#9372=CARTESIAN_POINT('',(25.,-3.06161699786838E-15,4.));
#9373=CARTESIAN_POINT('Origin',(0.,0.,4.));
#9374=CARTESIAN_POINT('Origin',(-15.,1.57116660247941E-13,4.));
#9375=CARTESIAN_POINT('',(-12.,1.56749266208197E-13,4.));
#9376=CARTESIAN_POINT('Origin',(-15.,1.57116660247941E-13,4.));
#9377=CARTESIAN_POINT('',(-12.,1.56749266208197E-13,0.));
#9378=CARTESIAN_POINT('',(-12.,1.56749266208197E-13,4.));
#9379=CARTESIAN_POINT('Origin',(-15.,1.57116660247941E-13,0.));
#9380=CARTESIAN_POINT('Origin',(-1.04744440165294E-13,-15.,4.));
#9381=CARTESIAN_POINT('',(2.9999999999999,-15.,4.));
#9382=CARTESIAN_POINT('Origin',(-1.04744440165294E-13,-15.,4.));
#9383=CARTESIAN_POINT('',(2.9999999999999,-15.,0.));
#9384=CARTESIAN_POINT('',(2.9999999999999,-15.,4.));
#9385=CARTESIAN_POINT('Origin',(-1.04744440165294E-13,-15.,0.));
#9386=CARTESIAN_POINT('Origin',(15.,-5.2372220082647E-14,4.));
#9387=CARTESIAN_POINT('',(18.,-5.27396141223912E-14,4.));
#9388=CARTESIAN_POINT('Origin',(15.,-5.2372220082647E-14,4.));
#9389=CARTESIAN_POINT('',(18.,-5.27396141223912E-14,0.));
#9390=CARTESIAN_POINT('',(18.,-5.27396141223912E-14,4.));
#9391=CARTESIAN_POINT('Origin',(15.,-5.2372220082647E-14,0.));
#9392=CARTESIAN_POINT('Origin',(0.,15.,4.));
#9393=CARTESIAN_POINT('',(3.,15.,4.));
#9394=CARTESIAN_POINT('Origin',(0.,15.,4.));
#9395=CARTESIAN_POINT('',(3.,15.,0.));
#9396=CARTESIAN_POINT('',(3.,15.,4.));
#9397=CARTESIAN_POINT('Origin',(0.,15.,0.));
#9398=CARTESIAN_POINT('Origin',(0.,0.,4.));
#9399=CARTESIAN_POINT('',(9.5,-1.16341445918999E-15,4.));
#9400=CARTESIAN_POINT('Origin',(0.,0.,4.));
#9401=CARTESIAN_POINT('',(9.5,-1.16341445918999E-15,2.));
#9402=CARTESIAN_POINT('',(9.5,-1.16341445918999E-15,4.));
#9403=CARTESIAN_POINT('Origin',(0.,0.,2.));
#9404=CARTESIAN_POINT('Origin',(0.,0.,4.));
#9405=CARTESIAN_POINT('Origin',(0.,0.,0.));
#9406=CARTESIAN_POINT('Origin',(0.,0.,2.));
#9407=CARTESIAN_POINT('',(0.,0.,0.));
#9408=CARTESIAN_POINT('Origin',(0.,0.,5.));
#9409=CARTESIAN_POINT('',(5.,-6.12323399573677E-16,5.));
#9410=CARTESIAN_POINT('Origin',(0.,0.,5.));
#9411=CARTESIAN_POINT('',(5.,-6.12323399573677E-16,0.));
#9412=CARTESIAN_POINT('',(5.,-6.12323399573677E-16,5.));
#9413=CARTESIAN_POINT('Origin',(0.,0.,0.));
#9414=CARTESIAN_POINT('Origin',(0.,0.,5.));
#9415=CARTESIAN_POINT('',(9.5,-1.16341445918999E-15,5.55111512312578E-16));
#9416=CARTESIAN_POINT('Origin',(0.,0.,0.));
#9417=CARTESIAN_POINT('',(9.5,-1.16341445918999E-15,5.));
#9418=CARTESIAN_POINT('',(9.5,-1.16341445918999E-15,5.));
#9419=CARTESIAN_POINT('Origin',(0.,0.,5.));
#9420=CARTESIAN_POINT('Origin',(0.,0.,5.));
#9421=CARTESIAN_POINT('Origin',(0.,0.,0.));
#9422=CARTESIAN_POINT('',(0.,0.,0.));
#9423=CARTESIAN_POINT('Origin',(0.,0.,22.));
#9424=CARTESIAN_POINT('',(2.5,-3.06161699786838E-16,2.));
#9425=CARTESIAN_POINT('Origin',(0.,0.,2.));
#9426=CARTESIAN_POINT('',(2.5,-3.06161699786838E-16,22.));
#9427=CARTESIAN_POINT('',(2.5,-3.06161699786838E-16,22.));
#9428=CARTESIAN_POINT('Origin',(0.,0.,22.));
#9429=CARTESIAN_POINT('Origin',(0.,0.,2.));
#9430=CARTESIAN_POINT('',(1.73205080756887,-3.00000000000004,2.));
#9431=CARTESIAN_POINT('',(3.46410161513777,-7.54101367678791E-15,2.));
#9432=CARTESIAN_POINT('',(1.73205080756887,-3.00000000000004,2.));
#9433=CARTESIAN_POINT('',(1.73205080756885,3.00000000000006,2.));
#9434=CARTESIAN_POINT('',(3.46410161513777,-7.54101367678791E-15,2.));
#9435=CARTESIAN_POINT('',(-1.73205080756889,3.00000000000006,2.));
#9436=CARTESIAN_POINT('',(1.73205080756885,3.00000000000006,2.));
#9437=CARTESIAN_POINT('',(-3.46410161513781,-6.50677102219972E-15,2.));
#9438=CARTESIAN_POINT('',(-1.73205080756889,3.00000000000006,2.));
#9439=CARTESIAN_POINT('',(-1.73205080756891,-3.00000000000004,2.));
#9440=CARTESIAN_POINT('',(-3.46410161513781,-6.50677102219972E-15,2.));
#9441=CARTESIAN_POINT('',(-1.73205080756891,-3.00000000000004,2.));
#9442=CARTESIAN_POINT('Origin',(1.73205080756887,-3.00000000000004,2.));
#9443=CARTESIAN_POINT('',(1.73205080756887,-3.00000000000004,0.));
#9444=CARTESIAN_POINT('',(3.46410161513777,-7.54101367678791E-15,0.));
#9445=CARTESIAN_POINT('',(1.73205080756887,-3.00000000000004,0.));
#9446=CARTESIAN_POINT('',(3.46410161513777,-7.54101367678791E-15,2.));
#9447=CARTESIAN_POINT('',(1.73205080756887,-3.00000000000004,2.));
#9448=CARTESIAN_POINT('Origin',(3.46410161513777,-7.54101367678791E-15,
2.));
#9449=CARTESIAN_POINT('',(1.73205080756885,3.00000000000006,0.));
#9450=CARTESIAN_POINT('',(3.46410161513777,-7.54101367678791E-15,0.));
#9451=CARTESIAN_POINT('',(1.73205080756885,3.00000000000006,2.));
#9452=CARTESIAN_POINT('Origin',(1.73205080756885,3.00000000000006,2.));
#9453=CARTESIAN_POINT('',(-1.73205080756889,3.00000000000006,0.));
#9454=CARTESIAN_POINT('',(1.73205080756885,3.00000000000006,0.));
#9455=CARTESIAN_POINT('',(-1.73205080756889,3.00000000000006,2.));
#9456=CARTESIAN_POINT('Origin',(-1.73205080756889,3.00000000000006,2.));
#9457=CARTESIAN_POINT('',(-3.46410161513781,-6.50677102219972E-15,0.));
#9458=CARTESIAN_POINT('',(-1.73205080756889,3.00000000000006,0.));
#9459=CARTESIAN_POINT('',(-3.46410161513781,-6.50677102219972E-15,2.));
#9460=CARTESIAN_POINT('Origin',(-3.46410161513781,-6.50677102219972E-15,
2.));
#9461=CARTESIAN_POINT('',(-1.73205080756891,-3.00000000000004,0.));
#9462=CARTESIAN_POINT('',(-3.46410161513781,-6.50677102219972E-15,0.));
#9463=CARTESIAN_POINT('',(-1.73205080756891,-3.00000000000004,2.));
#9464=CARTESIAN_POINT('Origin',(-1.73205080756891,-3.00000000000004,2.));
#9465=CARTESIAN_POINT('',(-1.73205080756891,-3.00000000000004,0.));
#9466=CARTESIAN_POINT('Origin',(0.,0.,0.));
#9467=CARTESIAN_POINT('Origin',(0.,0.,22.));
#9468=CARTESIAN_POINT('',(0.,0.,0.));
#9469=CARTESIAN_POINT('Origin',(-4.1335320013656,6.79957634403871E-15,-6.66133814775094E-15));
#9470=CARTESIAN_POINT('',(-0.696032001365594,7.11183652464788E-15,2.549797875));
#9471=CARTESIAN_POINT('',(-0.571032001365594,7.11183652464788E-15,2.549797875));
#9472=CARTESIAN_POINT('',(-4.1335320013656,1.39114128686866E-14,2.54979787499999));
#9473=CARTESIAN_POINT('',(8.51787316660525E-16,1.09749718660244,-2.30151452933807));
#9474=CARTESIAN_POINT('Ctrl Pts',(-0.571032001365594,3.12260180609148E-16,
2.549797875));
#9475=CARTESIAN_POINT('Ctrl Pts',(-0.508532001365594,-1.0561608611351,2.549797875));
#9476=CARTESIAN_POINT('Ctrl Pts',(-0.446032001365594,-1.80297936806755,
1.80297936806755));
#9477=CARTESIAN_POINT('Ctrl Pts',(-0.383532001365594,-2.549797875,1.0561608611351));
#9478=CARTESIAN_POINT('Ctrl Pts',(-0.321032001365594,-2.549797875,4.68390270913721E-16));
#9479=CARTESIAN_POINT('Ctrl Pts',(-0.258532001365594,-2.549797875,-1.0561608611351));
#9480=CARTESIAN_POINT('Ctrl Pts',(-0.196032001365594,-1.80297936806755,
-1.80297936806755));
#9481=CARTESIAN_POINT('Ctrl Pts',(-0.133532001365594,-1.0561608611351,-2.549797875));
#9482=CARTESIAN_POINT('Ctrl Pts',(-0.0710320013655938,0.,-2.549797875));
#9483=CARTESIAN_POINT('Ctrl Pts',(-0.0368970038158504,0.576832774511702,
-2.549797875));
#9484=CARTESIAN_POINT('Ctrl Pts',(8.51787316660525E-16,1.09749718660244,
-2.30151452933807));
#9485=CARTESIAN_POINT('',(1.55011212503014E-14,2.40346423367414,-0.851368827714362));
#9486=CARTESIAN_POINT('Origin',(0.,6.79957634403871E-15,-6.66133814775094E-15));
#9487=CARTESIAN_POINT('Ctrl Pts',(-0.696032001365594,3.12260180609148E-16,
2.549797875));
#9488=CARTESIAN_POINT('Ctrl Pts',(-0.633532001365594,-1.0561608611351,2.549797875));
#9489=CARTESIAN_POINT('Ctrl Pts',(-0.571032001365594,-1.80297936806755,
1.80297936806755));
#9490=CARTESIAN_POINT('Ctrl Pts',(-0.508532001365594,-2.549797875,1.0561608611351));
#9491=CARTESIAN_POINT('Ctrl Pts',(-0.446032001365594,-2.549797875,4.68390270913721E-16));
#9492=CARTESIAN_POINT('Ctrl Pts',(-0.383532001365594,-2.549797875,-1.0561608611351));
#9493=CARTESIAN_POINT('Ctrl Pts',(-0.321032001365594,-1.80297936806755,
-1.80297936806755));
#9494=CARTESIAN_POINT('Ctrl Pts',(-0.258532001365594,-1.0561608611351,-2.549797875));
#9495=CARTESIAN_POINT('Ctrl Pts',(-0.196032001365594,0.,-2.549797875));
#9496=CARTESIAN_POINT('Ctrl Pts',(-0.133532001365594,1.0561608611351,-2.549797875));
#9497=CARTESIAN_POINT('Ctrl Pts',(-0.0710320013655938,1.80297936806755,
-1.80297936806755));
#9498=CARTESIAN_POINT('Ctrl Pts',(-0.0368970038158433,2.21086173453551,
-1.39509700159959));
#9499=CARTESIAN_POINT('Ctrl Pts',(1.55011212503014E-14,2.40346423367414,
-0.851368827714362));
#9500=CARTESIAN_POINT('Origin',(-4.1335320013656,6.79957634403871E-15,-6.66133814775094E-15));
#9501=CARTESIAN_POINT('',(-1.69603200136559,7.11183652464788E-15,2.549797875));
#9502=CARTESIAN_POINT('',(-1.5710320013656,7.11183652464788E-15,2.549797875));
#9503=CARTESIAN_POINT('',(-4.1335320013656,1.39114128686866E-14,2.54979787499999));
#9504=CARTESIAN_POINT('Ctrl Pts',(-1.5710320013656,3.12260180609148E-16,
2.549797875));
#9505=CARTESIAN_POINT('Ctrl Pts',(-1.50853200136559,-1.0561608611351,2.549797875));
#9506=CARTESIAN_POINT('Ctrl Pts',(-1.44603200136559,-1.80297936806755,1.80297936806755));
#9507=CARTESIAN_POINT('Ctrl Pts',(-1.38353200136559,-2.549797875,1.0561608611351));
#9508=CARTESIAN_POINT('Ctrl Pts',(-1.32103200136559,-2.549797875,4.68390270913721E-16));
#9509=CARTESIAN_POINT('Ctrl Pts',(-1.2585320013656,-2.549797875,-1.0561608611351));
#9510=CARTESIAN_POINT('Ctrl Pts',(-1.19603200136559,-1.80297936806755,-1.80297936806755));
#9511=CARTESIAN_POINT('Ctrl Pts',(-1.13353200136559,-1.0561608611351,-2.549797875));
#9512=CARTESIAN_POINT('Ctrl Pts',(-1.07103200136559,0.,-2.549797875));
#9513=CARTESIAN_POINT('Ctrl Pts',(-1.00853200136559,1.0561608611351,-2.549797875));
#9514=CARTESIAN_POINT('Ctrl Pts',(-0.946032001365594,1.80297936806755,-1.80297936806755));
#9515=CARTESIAN_POINT('Ctrl Pts',(-0.883532001365593,2.549797875,-1.0561608611351));
#9516=CARTESIAN_POINT('Ctrl Pts',(-0.821032001365594,2.549797875,-1.56130090304574E-16));
#9517=CARTESIAN_POINT('Ctrl Pts',(-0.758532001365594,2.549797875,1.0561608611351));
#9518=CARTESIAN_POINT('Ctrl Pts',(-0.696032001365594,1.80297936806755,1.80297936806755));
#9519=CARTESIAN_POINT('Ctrl Pts',(-0.633532001365594,1.0561608611351,2.549797875));
#9520=CARTESIAN_POINT('Ctrl Pts',(-0.571032001365594,3.12260180609148E-16,
2.549797875));
#9521=CARTESIAN_POINT('Ctrl Pts',(-1.69603200136559,3.12260180609148E-16,
2.549797875));
#9522=CARTESIAN_POINT('Ctrl Pts',(-1.63353200136559,-1.0561608611351,2.549797875));
#9523=CARTESIAN_POINT('Ctrl Pts',(-1.5710320013656,-1.80297936806755,1.80297936806755));
#9524=CARTESIAN_POINT('Ctrl Pts',(-1.50853200136559,-2.549797875,1.0561608611351));
#9525=CARTESIAN_POINT('Ctrl Pts',(-1.44603200136559,-2.549797875,4.68390270913721E-16));
#9526=CARTESIAN_POINT('Ctrl Pts',(-1.38353200136559,-2.549797875,-1.0561608611351));
#9527=CARTESIAN_POINT('Ctrl Pts',(-1.32103200136559,-1.80297936806755,-1.80297936806755));
#9528=CARTESIAN_POINT('Ctrl Pts',(-1.2585320013656,-1.0561608611351,-2.549797875));
#9529=CARTESIAN_POINT('Ctrl Pts',(-1.19603200136559,0.,-2.549797875));
#9530=CARTESIAN_POINT('Ctrl Pts',(-1.13353200136559,1.0561608611351,-2.549797875));
#9531=CARTESIAN_POINT('Ctrl Pts',(-1.07103200136559,1.80297936806755,-1.80297936806755));
#9532=CARTESIAN_POINT('Ctrl Pts',(-1.00853200136559,2.549797875,-1.0561608611351));
#9533=CARTESIAN_POINT('Ctrl Pts',(-0.946032001365594,2.549797875,-1.56130090304574E-16));
#9534=CARTESIAN_POINT('Ctrl Pts',(-0.883532001365594,2.549797875,1.0561608611351));
#9535=CARTESIAN_POINT('Ctrl Pts',(-0.821032001365594,1.80297936806755,1.80297936806755));
#9536=CARTESIAN_POINT('Ctrl Pts',(-0.758532001365594,1.0561608611351,2.549797875));
#9537=CARTESIAN_POINT('Ctrl Pts',(-0.696032001365594,3.12260180609148E-16,
2.549797875));
#9538=CARTESIAN_POINT('Origin',(-4.1335320013656,6.79957634403871E-15,-6.66133814775094E-15));
#9539=CARTESIAN_POINT('',(-2.6960320013656,7.11183652464788E-15,2.549797875));
#9540=CARTESIAN_POINT('',(-2.5710320013656,7.11183652464788E-15,2.549797875));
#9541=CARTESIAN_POINT('',(-4.1335320013656,1.39114128686866E-14,2.54979787499999));
#9542=CARTESIAN_POINT('Ctrl Pts',(-2.5710320013656,3.12260180609148E-16,
2.549797875));
#9543=CARTESIAN_POINT('Ctrl Pts',(-2.5085320013656,-1.0561608611351,2.549797875));
#9544=CARTESIAN_POINT('Ctrl Pts',(-2.44603200136559,-1.80297936806755,1.80297936806755));
#9545=CARTESIAN_POINT('Ctrl Pts',(-2.38353200136559,-2.549797875,1.0561608611351));
#9546=CARTESIAN_POINT('Ctrl Pts',(-2.3210320013656,-2.549797875,4.68390270913721E-16));
#9547=CARTESIAN_POINT('Ctrl Pts',(-2.25853200136559,-2.549797875,-1.0561608611351));
#9548=CARTESIAN_POINT('Ctrl Pts',(-2.1960320013656,-1.80297936806755,-1.80297936806755));
#9549=CARTESIAN_POINT('Ctrl Pts',(-2.13353200136559,-1.0561608611351,-2.549797875));
#9550=CARTESIAN_POINT('Ctrl Pts',(-2.07103200136559,0.,-2.549797875));
#9551=CARTESIAN_POINT('Ctrl Pts',(-2.00853200136559,1.0561608611351,-2.549797875));
#9552=CARTESIAN_POINT('Ctrl Pts',(-1.9460320013656,1.80297936806755,-1.80297936806755));
#9553=CARTESIAN_POINT('Ctrl Pts',(-1.8835320013656,2.549797875,-1.0561608611351));
#9554=CARTESIAN_POINT('Ctrl Pts',(-1.82103200136559,2.549797875,-1.56130090304574E-16));
#9555=CARTESIAN_POINT('Ctrl Pts',(-1.7585320013656,2.549797875,1.0561608611351));
#9556=CARTESIAN_POINT('Ctrl Pts',(-1.69603200136559,1.80297936806755,1.80297936806755));
#9557=CARTESIAN_POINT('Ctrl Pts',(-1.63353200136559,1.0561608611351,2.549797875));
#9558=CARTESIAN_POINT('Ctrl Pts',(-1.5710320013656,3.12260180609148E-16,
2.549797875));
#9559=CARTESIAN_POINT('Ctrl Pts',(-2.6960320013656,3.12260180609148E-16,
2.549797875));
#9560=CARTESIAN_POINT('Ctrl Pts',(-2.6335320013656,-1.0561608611351,2.549797875));
#9561=CARTESIAN_POINT('Ctrl Pts',(-2.5710320013656,-1.80297936806755,1.80297936806755));
#9562=CARTESIAN_POINT('Ctrl Pts',(-2.5085320013656,-2.549797875,1.0561608611351));
#9563=CARTESIAN_POINT('Ctrl Pts',(-2.44603200136559,-2.549797875,4.68390270913721E-16));
#9564=CARTESIAN_POINT('Ctrl Pts',(-2.38353200136559,-2.549797875,-1.0561608611351));
#9565=CARTESIAN_POINT('Ctrl Pts',(-2.3210320013656,-1.80297936806755,-1.80297936806755));
#9566=CARTESIAN_POINT('Ctrl Pts',(-2.25853200136559,-1.0561608611351,-2.549797875));
#9567=CARTESIAN_POINT('Ctrl Pts',(-2.1960320013656,0.,-2.549797875));
#9568=CARTESIAN_POINT('Ctrl Pts',(-2.13353200136559,1.0561608611351,-2.549797875));
#9569=CARTESIAN_POINT('Ctrl Pts',(-2.07103200136559,1.80297936806755,-1.80297936806755));
#9570=CARTESIAN_POINT('Ctrl Pts',(-2.00853200136559,2.549797875,-1.0561608611351));
#9571=CARTESIAN_POINT('Ctrl Pts',(-1.9460320013656,2.549797875,-1.56130090304574E-16));
#9572=CARTESIAN_POINT('Ctrl Pts',(-1.8835320013656,2.549797875,1.0561608611351));
#9573=CARTESIAN_POINT('Ctrl Pts',(-1.82103200136559,1.80297936806755,1.80297936806755));
#9574=CARTESIAN_POINT('Ctrl Pts',(-1.7585320013656,1.0561608611351,2.549797875));
#9575=CARTESIAN_POINT('Ctrl Pts',(-1.69603200136559,3.12260180609148E-16,
2.549797875));
#9576=CARTESIAN_POINT('Origin',(-4.1335320013656,6.79957634403871E-15,-6.66133814775094E-15));
#9577=CARTESIAN_POINT('',(-3.6960320013656,7.11183652464788E-15,2.549797875));
#9578=CARTESIAN_POINT('',(-3.57103200136559,7.11183652464788E-15,2.549797875));
#9579=CARTESIAN_POINT('',(-4.1335320013656,1.39114128686866E-14,2.54979787499999));
#9580=CARTESIAN_POINT('',(-4.,2.40346423367405,-0.851368827714594));
#9581=CARTESIAN_POINT('Ctrl Pts',(-4.,2.40346423367405,-0.851368827714594));
#9582=CARTESIAN_POINT('Ctrl Pts',(-3.97196675564161,2.549797875,-0.438260358551676));
#9583=CARTESIAN_POINT('Ctrl Pts',(-3.9460320013656,2.549797875,-1.56130090304574E-16));
#9584=CARTESIAN_POINT('Ctrl Pts',(-3.88353200136559,2.549797875,1.0561608611351));
#9585=CARTESIAN_POINT('Ctrl Pts',(-3.8210320013656,1.80297936806755,1.80297936806755));
#9586=CARTESIAN_POINT('Ctrl Pts',(-3.75853200136559,1.0561608611351,2.549797875));
#9587=CARTESIAN_POINT('Ctrl Pts',(-3.6960320013656,3.12260180609148E-16,
2.549797875));
#9588=CARTESIAN_POINT('',(-4.,1.09749718660243,-2.30151452933807));
#9589=CARTESIAN_POINT('Origin',(-4.,6.79957634403871E-15,-6.66133814775094E-15));
#9590=CARTESIAN_POINT('Ctrl Pts',(-4.,1.09749718660243,-2.30151452933807));
#9591=CARTESIAN_POINT('Ctrl Pts',(-3.97196675564161,1.49308249661042,-2.11287623952468));
#9592=CARTESIAN_POINT('Ctrl Pts',(-3.9460320013656,1.80297936806755,-1.80297936806755));
#9593=CARTESIAN_POINT('Ctrl Pts',(-3.88353200136559,2.549797875,-1.0561608611351));
#9594=CARTESIAN_POINT('Ctrl Pts',(-3.8210320013656,2.549797875,-1.56130090304574E-16));
#9595=CARTESIAN_POINT('Ctrl Pts',(-3.75853200136559,2.549797875,1.0561608611351));
#9596=CARTESIAN_POINT('Ctrl Pts',(-3.6960320013656,1.80297936806755,1.80297936806755));
#9597=CARTESIAN_POINT('Ctrl Pts',(-3.63353200136559,1.0561608611351,2.549797875));
#9598=CARTESIAN_POINT('Ctrl Pts',(-3.57103200136559,3.12260180609148E-16,
2.549797875));
#9599=CARTESIAN_POINT('Origin',(-3.508532,0.,0.));
#9600=CARTESIAN_POINT('',(-3.508532,0.,-2.008532));
#9601=CARTESIAN_POINT('',(-4.00000000000008,-3.06161699786848E-16,-2.50000000000008));
#9602=CARTESIAN_POINT('',(-3.508532,-2.45974228478503E-16,-2.008532));
#9603=CARTESIAN_POINT('',(-3.508532,2.008532,3.63558707729711E-8));
#9604=CARTESIAN_POINT('Origin',(-3.508532,0.,0.));
#9605=CARTESIAN_POINT('',(-4.,0.663411757904749,-2.41037027020201));
#9606=CARTESIAN_POINT('Ctrl Pts',(-3.50853200000001,2.00853200000001,3.6355872479677E-8));
#9607=CARTESIAN_POINT('Ctrl Pts',(-3.53382612947289,2.03382613204873,-0.142306019496749));
#9608=CARTESIAN_POINT('Ctrl Pts',(-3.57736045030338,2.06353600790935,-0.386343636106257));
#9609=CARTESIAN_POINT('Ctrl Pts',(-3.67936504533042,1.97724583342445,-0.952917190711209));
#9610=CARTESIAN_POINT('Ctrl Pts',(-3.7250839713689,1.88868644811177,-1.20522505423621));
#9611=CARTESIAN_POINT('Ctrl Pts',(-3.78543276629123,1.70131965479837,-1.52981386634904));
#9612=CARTESIAN_POINT('Ctrl Pts',(-3.8042150333194,1.63228546614519,-1.63220361975085));
#9613=CARTESIAN_POINT('Ctrl Pts',(-3.85459829755779,1.42567390080877,-1.88282757659245));
#9614=CARTESIAN_POINT('Ctrl Pts',(-3.8838183841557,1.29197929165672,-2.01166246391125));
#9615=CARTESIAN_POINT('Ctrl Pts',(-3.94240582504991,0.996071238886274,-2.23772216093148));
#9616=CARTESIAN_POINT('Ctrl Pts',(-3.97157997728534,0.834519750270115,-2.33379900101778));
#9617=CARTESIAN_POINT('Ctrl Pts',(-4.00000000000008,0.663411757904799,-2.41037027020209));
#9618=CARTESIAN_POINT('Origin',(-4.,0.,0.));
#9619=CARTESIAN_POINT('Origin',(0.,0.,0.));
#9620=CARTESIAN_POINT('',(-0.343792495187435,-1.84798906267329E-17,2.15620750481256));
#9621=CARTESIAN_POINT('',(2.39626859034904E-16,-3.06161699786838E-16,2.5));
#9622=CARTESIAN_POINT('',(0.,-3.06161699786838E-16,2.5));
#9623=CARTESIAN_POINT('',(-0.491468,1.99622053939136,0.222045835664713));
#9624=CARTESIAN_POINT('Ctrl Pts',(-0.343792495187436,2.27099480653155E-16,
2.15620750481256));
#9625=CARTESIAN_POINT('Ctrl Pts',(-0.346835563302273,0.068592189879008,
2.15316443669773));
#9626=CARTESIAN_POINT('Ctrl Pts',(-0.349953972956135,0.137232557864158,
2.14676612902208));
#9627=CARTESIAN_POINT('Ctrl Pts',(-0.365326801994469,0.467558433699237,
2.09956409034472));
#9628=CARTESIAN_POINT('Ctrl Pts',(-0.378214054572241,0.720278039460965,
2.01322828587724));
#9629=CARTESIAN_POINT('Ctrl Pts',(-0.397835304293012,1.06917445992625,1.8150899345924));
#9630=CARTESIAN_POINT('Ctrl Pts',(-0.404478939263286,1.18106791295702,1.73634110638149));
#9631=CARTESIAN_POINT('Ctrl Pts',(-0.422639367746322,1.46966390990759,1.4882674492164));
#9632=CARTESIAN_POINT('Ctrl Pts',(-0.43507971277735,1.65099064940197,1.27684962103764));
#9633=CARTESIAN_POINT('Ctrl Pts',(-0.457107777658471,1.84707317679396,0.883230819666249));
#9634=CARTESIAN_POINT('Ctrl Pts',(-0.4640029816804,1.8952762649122,0.756026772227834));
#9635=CARTESIAN_POINT('Ctrl Pts',(-0.477826971755898,1.96583127251109,0.493210297151591));
#9636=CARTESIAN_POINT('Ctrl Pts',(-0.484720391457909,1.98786166530542,0.358229176938792));
#9637=CARTESIAN_POINT('Ctrl Pts',(-0.491468,1.99622053939137,0.222045835664711));
#9638=CARTESIAN_POINT('',(-0.49146799999999,0.222045800910263,-1.99622054325721));
#9639=CARTESIAN_POINT('Origin',(-0.491468,0.,0.));
#9640=CARTESIAN_POINT('',(2.36346660700959E-16,2.46710998658661,-0.404188463571893));
#9641=CARTESIAN_POINT('Ctrl Pts',(-0.491467999999976,0.22204580091026,-1.99622054325724));
#9642=CARTESIAN_POINT('Ctrl Pts',(-0.448230267693132,0.459369200980115,
-2.0133267215389));
#9643=CARTESIAN_POINT('Ctrl Pts',(-0.404633819457699,0.697802895750879,
-1.98960723762313));
#9644=CARTESIAN_POINT('Ctrl Pts',(-0.297858721744298,1.27716376442399,-1.82918786458872));
#9645=CARTESIAN_POINT('Ctrl Pts',(-0.253226754599606,1.51258806051641,-1.66615397659853));
#9646=CARTESIAN_POINT('Ctrl Pts',(-0.195036445899189,1.81238247207411,-1.44449973647153));
#9647=CARTESIAN_POINT('Ctrl Pts',(-0.155671364837018,1.98548385608536,-1.26966634451936));
#9648=CARTESIAN_POINT('Ctrl Pts',(-0.0765988208212301,2.27597002415698,
-0.868392304059463));
#9649=CARTESIAN_POINT('Ctrl Pts',(-0.0373743863901998,2.39007414194648,
-0.643235206290509));
#9650=CARTESIAN_POINT('Ctrl Pts',(-6.67868538251071E-16,2.46710998658661,
-0.404188463571894));
#9651=CARTESIAN_POINT('Origin',(0.,0.,0.));
#9652=CARTESIAN_POINT('Origin',(0.,0.,0.));
#9653=CARTESIAN_POINT('',(-2.50853200000007,-4.84827408638443E-13,-2.008532));
#9654=CARTESIAN_POINT('',(-2.75853200273112,4.5044732021816E-13,-2.008532));
#9655=CARTESIAN_POINT('',(0.,-2.45974228478503E-16,-2.008532));
#9656=CARTESIAN_POINT('Ctrl Pts',(-2.75853200273112,9.01084762361393E-13,
-2.008532));
#9657=CARTESIAN_POINT('Ctrl Pts',(-2.77456055212585,-0.213362097700962,
-2.008532));
#9658=CARTESIAN_POINT('Ctrl Pts',(-2.79156461992547,-0.425632430784419,
-1.97454648813002));
#9659=CARTESIAN_POINT('Ctrl Pts',(-2.83007698894459,-0.876690264569696,
-1.82584321873764));
#9660=CARTESIAN_POINT('Ctrl Pts',(-2.85134459536468,-1.10626401391303,-1.69661658903667));
#9661=CARTESIAN_POINT('Ctrl Pts',(-2.8919216544136,-1.50521292752755,-1.35575932192851));
#9662=CARTESIAN_POINT('Ctrl Pts',(-2.9118599566143,-1.67003511935622,-1.1466282571683));
#9663=CARTESIAN_POINT('Ctrl Pts',(-2.95440287010154,-1.90822520426924,-0.678984970559192));
#9664=CARTESIAN_POINT('Ctrl Pts',(-2.97568935673053,-1.98024302784687,-0.425463236213872));
#9665=CARTESIAN_POINT('Ctrl Pts',(-3.0163093462195,-2.02340063934787,0.0973683756301305));
#9666=CARTESIAN_POINT('Ctrl Pts',(-3.03618042320102,-1.99319715537815,0.361686706262085));
#9667=CARTESIAN_POINT('Ctrl Pts',(-3.07869865966288,-1.83315117101439,0.86136985389795));
#9668=CARTESIAN_POINT('Ctrl Pts',(-3.10000450055328,-1.7057348138004,1.09220239618666));
#9669=CARTESIAN_POINT('Ctrl Pts',(-3.14066896724781,-1.36830702982799,1.49373536453641));
#9670=CARTESIAN_POINT('Ctrl Pts',(-3.16047214757596,-1.16095821365585,1.66003135284234));
#9671=CARTESIAN_POINT('Ctrl Pts',(-3.20296419129915,-0.695657166562376,
1.90224132737754));
#9672=CARTESIAN_POINT('Ctrl Pts',(-3.22428981667312,-0.442552167990885,
1.97652302286004));
#9673=CARTESIAN_POINT('Ctrl Pts',(-3.26500027165569,0.079646828549336,2.02411514822785));
#9674=CARTESIAN_POINT('Ctrl Pts',(-3.28473516831841,0.343737016683785,1.99630822223585));
#9675=CARTESIAN_POINT('Ctrl Pts',(-3.32719944636982,0.84464396057714,1.84095077849946));
#9676=CARTESIAN_POINT('Ctrl Pts',(-3.34854523630185,1.07682912175842,1.71551610930506));
#9677=CARTESIAN_POINT('Ctrl Pts',(-3.38930314393295,1.48115404399385,1.38182583248953));
#9678=CARTESIAN_POINT('Ctrl Pts',(-3.40896968143032,1.64904253759952,1.17640639382414));
#9679=CARTESIAN_POINT('Ctrl Pts',(-3.44364132718139,1.85048763662499,0.798320264684737));
#9680=CARTESIAN_POINT('Ctrl Pts',(-3.45715263173166,1.90998221265315,0.643109627718993));
#9681=CARTESIAN_POINT('Ctrl Pts',(-3.48354365253707,1.98881459742706,0.324462187400849));
#9682=CARTESIAN_POINT('Ctrl Pts',(-3.49632501857545,2.00853199705883,0.162491792763301));
#9683=CARTESIAN_POINT('Ctrl Pts',(-3.50853200000005,2.008532,3.63552882937102E-8));
#9684=CARTESIAN_POINT('Ctrl Pts',(-3.50853200000007,-9.84420878147318E-13,
-2.008532));
#9685=CARTESIAN_POINT('Ctrl Pts',(-3.49046402821612,0.24050962230436,-2.00853200000012));
#9686=CARTESIAN_POINT('Ctrl Pts',(-3.47118913480691,0.479191425417207,-1.96533300281851));
#9687=CARTESIAN_POINT('Ctrl Pts',(-3.43195318010694,0.931316582506389,-1.79595295990627));
#9688=CARTESIAN_POINT('Ctrl Pts',(-3.41231741129813,1.1408277657495,-1.67073258000721));
#9689=CARTESIAN_POINT('Ctrl Pts',(-3.37380973218154,1.51700588350948,-1.34140440174912));
#9690=CARTESIAN_POINT('Ctrl Pts',(-3.35418898308051,1.67650575064658,-1.13579659149845));
#9691=CARTESIAN_POINT('Ctrl Pts',(-3.31160830748131,1.91328256950635,-0.667065245134157));
#9692=CARTESIAN_POINT('Ctrl Pts',(-3.28982593566044,1.98498673948956,-0.406812675428285));
#9693=CARTESIAN_POINT('Ctrl Pts',(-3.24933193849708,2.02162373382201,0.117042732869852));
#9694=CARTESIAN_POINT('Ctrl Pts',(-3.22975941185735,1.98993503616935,0.37529971433039));
#9695=CARTESIAN_POINT('Ctrl Pts',(-3.18720029581631,1.82772911320931,0.874632349682423));
#9696=CARTESIAN_POINT('Ctrl Pts',(-3.16541623828598,1.69530469933909,1.10975620997746));
#9697=CARTESIAN_POINT('Ctrl Pts',(-3.12488147033888,1.35233179291034,1.50726584420255));
#9698=CARTESIAN_POINT('Ctrl Pts',(-3.10535792486904,1.14792370883617,1.66821748998151));
#9699=CARTESIAN_POINT('Ctrl Pts',(-3.06282169833356,0.681147963820842,1.9082871102709));
#9700=CARTESIAN_POINT('Ctrl Pts',(-3.04103617811804,0.421629789606673,1.98186544623294));
#9701=CARTESIAN_POINT('Ctrl Pts',(-3.00045894616575,-0.101698818431005,
2.02244912469178));
#9702=CARTESIAN_POINT('Ctrl Pts',(-2.98098493355571,-0.360143118773108,
1.99272777038104));
#9703=CARTESIAN_POINT('Ctrl Pts',(-2.93847298163481,-0.860460138050051,
1.83441405075633));
#9704=CARTESIAN_POINT('Ctrl Pts',(-2.91668626529548,-1.0964215950684,1.70392632940774));
#9705=CARTESIAN_POINT('Ctrl Pts',(-2.87606489189739,-1.49645967791858,1.36427444082656));
#9706=CARTESIAN_POINT('Ctrl Pts',(-2.85664073019463,-1.65900786950074,1.16118486715188));
#9707=CARTESIAN_POINT('Ctrl Pts',(-2.81415449127765,-1.90268273496045,0.69656786772297));
#9708=CARTESIAN_POINT('Ctrl Pts',(-2.79236689209776,-1.97831101929844,0.437871136045353));
#9709=CARTESIAN_POINT('Ctrl Pts',(-2.75169972683183,-2.02322266864599,-0.0848619041858379));
#9710=CARTESIAN_POINT('Ctrl Pts',(-2.73232547388737,-1.99565758636962,-0.343512247713487));
#9711=CARTESIAN_POINT('Ctrl Pts',(-2.6898664370209,-1.84160494767054,-0.84488989214959));
#9712=CARTESIAN_POINT('Ctrl Pts',(-2.66807831795509,-1.71324244732735,-1.08175031675541));
#9713=CARTESIAN_POINT('Ctrl Pts',(-2.62736374935824,-1.37723452127275,-1.48453833492761));
#9714=CARTESIAN_POINT('Ctrl Pts',(-2.6080391768759,-1.17558488172237,-1.64883138142115));
#9715=CARTESIAN_POINT('Ctrl Pts',(-2.56560887833205,-0.713336568558181,
-1.8964270329139));
#9716=CARTESIAN_POINT('Ctrl Pts',(-2.54382065462528,-0.455553842404719,
-1.97428199190002));
#9717=CARTESIAN_POINT('Ctrl Pts',(-2.51815002732461,-0.126787411536768,
-2.00553403794086));
#9718=CARTESIAN_POINT('Ctrl Pts',(-2.51329191108178,-0.0633609809763618,
-2.00853199999997));
#9719=CARTESIAN_POINT('Ctrl Pts',(-2.50853200000007,-9.69408843048408E-13,
-2.008532));
#9720=CARTESIAN_POINT('Origin',(0.,0.,0.));
#9721=CARTESIAN_POINT('',(-1.50853200000003,-1.87893736619935E-13,-2.008532));
#9722=CARTESIAN_POINT('',(-1.75853200273116,1.91028052360107E-13,-2.008532));
#9723=CARTESIAN_POINT('',(0.,-2.45974228478503E-16,-2.008532));
#9724=CARTESIAN_POINT('Ctrl Pts',(-1.75853200273116,3.82471831983366E-13,
-2.008532));
#9725=CARTESIAN_POINT('Ctrl Pts',(-1.77537323605212,-0.224180041546037,
-2.008532));
#9726=CARTESIAN_POINT('Ctrl Pts',(-1.79327970945474,-0.446997704203966,
-1.97100982574499));
#9727=CARTESIAN_POINT('Ctrl Pts',(-1.83325007951551,-0.912115609212472,
-1.80939550301654));
#9728=CARTESIAN_POINT('Ctrl Pts',(-1.85502063478529,-1.14493359087161,-1.67183812122849));
#9729=CARTESIAN_POINT('Ctrl Pts',(-1.89531797748143,-1.53563528603391,-1.32005941540903));
#9730=CARTESIAN_POINT('Ctrl Pts',(-1.9151454613833,-1.69232269859826,-1.11212547518953));
#9731=CARTESIAN_POINT('Ctrl Pts',(-1.95780947951013,-1.92268217297538,-0.639626573724209));
#9732=CARTESIAN_POINT('Ctrl Pts',(-1.97958232170033,-1.99072930021264,-0.377986059841389));
#9733=CARTESIAN_POINT('Ctrl Pts',(-2.02046371196938,-2.02008838063642,0.154040695600997));
#9734=CARTESIAN_POINT('Ctrl Pts',(-2.04083576575705,-1.98214662124489,0.419078454838985));
#9735=CARTESIAN_POINT('Ctrl Pts',(-2.08351416665944,-1.80704520927283,0.914657449761193));
#9736=CARTESIAN_POINT('Ctrl Pts',(-2.1046801365488,-1.67335278521896,1.14102848412408));
#9737=CARTESIAN_POINT('Ctrl Pts',(-2.14503284668744,-1.32396908043453,1.53345923821485));
#9738=CARTESIAN_POINT('Ctrl Pts',(-2.16534800272504,-1.11035708368627,1.69456239610697));
#9739=CARTESIAN_POINT('Ctrl Pts',(-2.20801059996808,-0.636915298361913,
1.9225998852347));
#9740=CARTESIAN_POINT('Ctrl Pts',(-2.22919202191717,-0.382435752508305,
1.98892893493238));
#9741=CARTESIAN_POINT('Ctrl Pts',(-2.26957817706242,0.141904562212205,2.02092959529444));
#9742=CARTESIAN_POINT('Ctrl Pts',(-2.28983454425305,0.406789812894553,1.98465498207741));
#9743=CARTESIAN_POINT('Ctrl Pts',(-2.33248025777436,0.903272599338705,1.81278597426953));
#9744=CARTESIAN_POINT('Ctrl Pts',(-2.35367774482194,1.13061657281339,1.68042958148138));
#9745=CARTESIAN_POINT('Ctrl Pts',(-2.39409890772545,1.52501936204394,1.33360695757695));
#9746=CARTESIAN_POINT('Ctrl Pts',(-2.41429469159831,1.68724808803654,1.12134842182099));
#9747=CARTESIAN_POINT('Ctrl Pts',(-2.45692237988489,1.91835911857486,0.649644425387381));
#9748=CARTESIAN_POINT('Ctrl Pts',(-2.47813653527762,1.98640587517699,0.395440649751718));
#9749=CARTESIAN_POINT('Ctrl Pts',(-2.51859428604895,2.02177771589593,-0.128456312865644));
#9750=CARTESIAN_POINT('Ctrl Pts',(-2.53872781259309,1.98734394944944,-0.393171494941496));
#9751=CARTESIAN_POINT('Ctrl Pts',(-2.58133627155539,1.81905137160877,-0.890639777624114));
#9752=CARTESIAN_POINT('Ctrl Pts',(-2.60256768385786,1.6881805612415,-1.11905069141494));
#9753=CARTESIAN_POINT('Ctrl Pts',(-2.6430636129712,1.34419532529303,-1.51562400658278));
#9754=CARTESIAN_POINT('Ctrl Pts',(-2.66313335395705,1.13342870882672,-1.67909113971857));
#9755=CARTESIAN_POINT('Ctrl Pts',(-2.70572131623673,0.663653961037752,-1.91358313320274));
#9756=CARTESIAN_POINT('Ctrl Pts',(-2.72697055406582,0.409767730895626,-1.98352393957922));
#9757=CARTESIAN_POINT('Ctrl Pts',(-2.75098176054802,0.0997356834155793,
-2.00667679103208));
#9758=CARTESIAN_POINT('Ctrl Pts',(-2.75478766083053,0.0498423545863755,
-2.008532));
#9759=CARTESIAN_POINT('Ctrl Pts',(-2.75853200273112,9.01140614664799E-13,
-2.008532));
#9760=CARTESIAN_POINT('Ctrl Pts',(-2.50853200000007,-9.69432867314879E-13,
-2.008532));
#9761=CARTESIAN_POINT('Ctrl Pts',(-2.49399315289905,0.193532105696083,-2.00853200000009));
#9762=CARTESIAN_POINT('Ctrl Pts',(-2.47863992207159,0.386323202437939,-1.98057159372929));
#9763=CARTESIAN_POINT('Ctrl Pts',(-2.44138171048376,0.827895436688843,-1.8492723066343));
#9764=CARTESIAN_POINT('Ctrl Pts',(-2.41959385185823,1.06571197843661,-1.72322644690499));
#9765=CARTESIAN_POINT('Ctrl Pts',(-2.37877986112267,1.47146879642677,-1.39119075688095));
#9766=CARTESIAN_POINT('Ctrl Pts',(-2.35955269820111,1.63765593032482,-1.1911029144753));
#9767=CARTESIAN_POINT('Ctrl Pts',(-2.31718465159873,1.88948442789464,-0.731436562757464));
#9768=CARTESIAN_POINT('Ctrl Pts',(-2.29539768390315,1.96973980952704,-0.474664843460665));
#9769=CARTESIAN_POINT('Ctrl Pts',(-2.25453181651249,2.02446596771235,0.0466478934158013));
#9770=CARTESIAN_POINT('Ctrl Pts',(-2.23535169477563,2.00178748462765,0.305768161170202));
#9771=CARTESIAN_POINT('Ctrl Pts',(-2.19301723102606,1.85737034409159,0.809478719638799));
#9772=CARTESIAN_POINT('Ctrl Pts',(-2.17123173724092,1.7338315431404,1.04830223984719));
#9773=CARTESIAN_POINT('Ctrl Pts',(-2.13031266638767,1.40609525397113,1.45723868926572));
#9774=CARTESIAN_POINT('Ctrl Pts',(-2.11117798753703,1.20768891749111,1.6254669535037));
#9775=CARTESIAN_POINT('Ctrl Pts',(-2.06887877944622,0.750816893465448,1.88182932523272));
#9776=CARTESIAN_POINT('Ctrl Pts',(-2.04709539994176,0.495156108327564,1.96465142723139));
#9777=CARTESIAN_POINT('Ctrl Pts',(-2.00612190301594,-0.0253221998097055,
2.02485091244375));
#9778=CARTESIAN_POINT('Ctrl Pts',(-1.98703068448704,-0.284706281507777,
2.00489648210646));
#9779=CARTESIAN_POINT('Ctrl Pts',(-1.9450715752669,-0.786052589074438,1.86683412031729));
#9780=CARTESIAN_POINT('Ctrl Pts',(-1.92360030332328,-1.02280145255032,1.74838464892588));
#9781=CARTESIAN_POINT('Ctrl Pts',(-1.88253079898025,-1.43667772949327,1.4277397507126));
#9782=CARTESIAN_POINT('Ctrl Pts',(-1.86325589841118,-1.6100205411952,1.22895066344172));
#9783=CARTESIAN_POINT('Ctrl Pts',(-1.82103392456302,-1.87139489634744,0.775182765209177));
#9784=CARTESIAN_POINT('Ctrl Pts',(-1.79954171907214,-1.95655067049019,0.524364546407468));
#9785=CARTESIAN_POINT('Ctrl Pts',(-1.75841678561011,-2.0254198564022,0.00546151673586223));
#9786=CARTESIAN_POINT('Ctrl Pts',(-1.73920026493478,-2.00898958408763,-0.257521591994173));
#9787=CARTESIAN_POINT('Ctrl Pts',(-1.69702003124529,-1.87603869397377,-0.763928612096199));
#9788=CARTESIAN_POINT('Ctrl Pts',(-1.67550710708127,-1.76024404664785,-1.00233158820248));
#9789=CARTESIAN_POINT('Ctrl Pts',(-1.63432606389763,-1.4445089394228,-1.41972630295501));
#9790=CARTESIAN_POINT('Ctrl Pts',(-1.61516486190513,-1.24817429840401,-1.59508307320836));
#9791=CARTESIAN_POINT('Ctrl Pts',(-1.57302815681787,-0.797799720262673,
-1.86190938718852));
#9792=CARTESIAN_POINT('Ctrl Pts',(-1.55149481751584,-0.547724619970668,
-1.95018110533127));
#9793=CARTESIAN_POINT('Ctrl Pts',(-1.52318811370744,-0.192237777317641,
-2.00163867517231));
#9794=CARTESIAN_POINT('Ctrl Pts',(-1.51575009246435,-0.0960827653000358,
-2.00853199999998));
#9795=CARTESIAN_POINT('Ctrl Pts',(-1.50853200000003,-3.75541499011392E-13,
-2.008532));
#9796=CARTESIAN_POINT('Origin',(0.,0.,0.));
#9797=CARTESIAN_POINT('',(-0.508531999999968,2.08048577268714E-13,-2.008532));
#9798=CARTESIAN_POINT('',(-0.758532002731178,6.47213330337261E-14,-2.008532));
#9799=CARTESIAN_POINT('',(0.,-2.45974228478503E-16,-2.008532));
#9800=CARTESIAN_POINT('Ctrl Pts',(-0.508531999999968,4.16343128765906E-13,
-2.008532));
#9801=CARTESIAN_POINT('Ctrl Pts',(-0.50296733755124,0.074073331517712,-2.008532));
#9802=CARTESIAN_POINT('Ctrl Pts',(-0.497271803520675,0.148191934104109,
-2.00443553786825));
#9803=CARTESIAN_POINT('Ctrl Pts',(-0.49146799999999,0.222045800910263,-1.99622054325721));
#9804=CARTESIAN_POINT('Ctrl Pts',(-0.491467999999934,1.99622053939127,0.222045835665548));
#9805=CARTESIAN_POINT('Ctrl Pts',(-0.503500023483089,2.01325127151279,0.068937369749291));
#9806=CARTESIAN_POINT('Ctrl Pts',(-0.514833549485698,2.01261300279072,-0.085572684581587));
#9807=CARTESIAN_POINT('Ctrl Pts',(-0.539214417763003,1.9756272638048,-0.394795670738753));
#9808=CARTESIAN_POINT('Ctrl Pts',(-0.55189707065267,1.93863972224196,-0.548298530217973));
#9809=CARTESIAN_POINT('Ctrl Pts',(-0.586474880195251,1.79119618574373,-0.947503749599346));
#9810=CARTESIAN_POINT('Ctrl Pts',(-0.608223847068728,1.64877810702651,-1.17802099334014));
#9811=CARTESIAN_POINT('Ctrl Pts',(-0.648285515458815,1.28865128670949,-1.56212763622119));
#9812=CARTESIAN_POINT('Ctrl Pts',(-0.668456402771949,1.07733276611845,-1.7147277761548));
#9813=CARTESIAN_POINT('Ctrl Pts',(-0.711234900865904,0.599410782925871,
-1.9356737599134));
#9814=CARTESIAN_POINT('Ctrl Pts',(-0.732985768951428,0.335837238716916,
-1.99834796804225));
#9815=CARTESIAN_POINT('Ctrl Pts',(-0.755130222334065,0.0451250070225805,
-2.00815204740256));
#9816=CARTESIAN_POINT('Ctrl Pts',(-0.756837522219823,0.0225558724944502,
-2.008532));
#9817=CARTESIAN_POINT('Ctrl Pts',(-0.758532002731178,1.29688640295931E-13,
-2.008532));
#9818=CARTESIAN_POINT('Origin',(0.,0.,0.));
#9819=CARTESIAN_POINT('Ctrl Pts',(-0.758532002731179,1.29340982368831E-13,
-2.008532));
#9820=CARTESIAN_POINT('Ctrl Pts',(-0.776206629942389,-0.235273663573603,
-2.008532));
#9821=CARTESIAN_POINT('Ctrl Pts',(-0.795044682083602,-0.468914196920289,
-1.96720085563323));
#9822=CARTESIAN_POINT('Ctrl Pts',(-0.835979030048088,-0.942081937442259,
-1.7940416675059));
#9823=CARTESIAN_POINT('Ctrl Pts',(-0.857731872939479,-1.17295963346949,
-1.65236923589102));
#9824=CARTESIAN_POINT('Ctrl Pts',(-0.897830394354453,-1.55808762843327,
-1.29352384994752));
#9825=CARTESIAN_POINT('Ctrl Pts',(-0.917945023665489,-1.7113181533755,-1.08272761527968));
#9826=CARTESIAN_POINT('Ctrl Pts',(-0.960706386238093,-1.93372256231143,
-0.605637828996343));
#9827=CARTESIAN_POINT('Ctrl Pts',(-0.982461274020495,-1.99722972218349,
-0.342355796987144));
#9828=CARTESIAN_POINT('Ctrl Pts',(-1.0225799633235,-2.01670908902974,0.183610668098889));
#9829=CARTESIAN_POINT('Ctrl Pts',(-1.04266419617014,-1.97645171555318,0.441058478084166));
#9830=CARTESIAN_POINT('Ctrl Pts',(-1.08541606380662,-1.79725151794042,0.935917643954678));
#9831=CARTESIAN_POINT('Ctrl Pts',(-1.10717306177851,-1.65642642852138,1.16720163046321));
#9832=CARTESIAN_POINT('Ctrl Pts',(-1.14731315213468,-1.29903685763934,1.55348598370563));
#9833=CARTESIAN_POINT('Ctrl Pts',(-1.16736543584026,-1.08883275610851,1.70743133606404));
#9834=CARTESIAN_POINT('Ctrl Pts',(-1.21010713618721,-0.612688535434477,
1.93148666696733));
#9835=CARTESIAN_POINT('Ctrl Pts',(-1.2318663034081,-0.349740010443477,1.9959365102324));
#9836=CARTESIAN_POINT('Ctrl Pts',(-1.2720290820139,0.175999334796381,2.01738106929987));
#9837=CARTESIAN_POINT('Ctrl Pts',(-1.29204784227751,0.433539482549909,1.97810671882581));
#9838=CARTESIAN_POINT('Ctrl Pts',(-1.3347786597579,0.928927240966364,1.8008591350999));
#9839=CARTESIAN_POINT('Ctrl Pts',(-1.35654004741073,1.16066745678154,1.66099441162635));
#9840=CARTESIAN_POINT('Ctrl Pts',(-1.3967268548385,1.54825693866292,1.30525437627347));
#9841=CARTESIAN_POINT('Ctrl Pts',(-1.41671050468876,1.7030105400602,1.09571963930088));
#9842=CARTESIAN_POINT('Ctrl Pts',(-1.45942967847865,1.92892885105761,0.620646949789437));
#9843=CARTESIAN_POINT('Ctrl Pts',(-1.4811933280373,1.99444217192984,0.358079265549406));
#9844=CARTESIAN_POINT('Ctrl Pts',(-1.52140555706854,2.01810610587264,-0.16739903787763));
#9845=CARTESIAN_POINT('Ctrl Pts',(-1.54135250729902,1.97994137375992,-0.425043553993443));
#9846=CARTESIAN_POINT('Ctrl Pts',(-1.58405922934413,1.80489703799285,-0.921023184121574));
#9847=CARTESIAN_POINT('Ctrl Pts',(-1.60582517053885,1.66611752328278,-1.15327352204698));
#9848=CARTESIAN_POINT('Ctrl Pts',(-1.64606426442597,1.31224090848214,-1.54233086287674));
#9849=CARTESIAN_POINT('Ctrl Pts',(-1.66597293560513,1.10346035458751,-1.69799538218072));
#9850=CARTESIAN_POINT('Ctrl Pts',(-1.70866634870659,0.629598297633439,-1.92600856004427));
#9851=CARTESIAN_POINT('Ctrl Pts',(-1.73043459728279,0.367464563231961,-1.99271732488473));
#9852=CARTESIAN_POINT('Ctrl Pts',(-1.75350189558004,0.0666147617554255,
-2.00770416246007));
#9853=CARTESIAN_POINT('Ctrl Pts',(-1.75603081447768,0.033294265087432,-2.008532));
#9854=CARTESIAN_POINT('Ctrl Pts',(-1.75853200273116,3.82302078948693E-13,
-2.008532));
#9855=CARTESIAN_POINT('Ctrl Pts',(-1.50853200000003,-3.75845188305135E-13,
-2.008532));
#9856=CARTESIAN_POINT('Ctrl Pts',(-1.4962584313927,0.163378124859691,-2.00853200000003));
#9857=CARTESIAN_POINT('Ctrl Pts',(-1.48338752376592,0.326453885797803,-1.98860563634782));
#9858=CARTESIAN_POINT('Ctrl Pts',(-1.44905636215842,0.740690958538574,-1.88537860842314));
#9859=CARTESIAN_POINT('Ctrl Pts',(-1.42750299973453,0.980791387042714,-1.77238242907389));
#9860=CARTESIAN_POINT('Ctrl Pts',(-1.38620827425788,1.40183226807111,-1.46179659354929));
#9861=CARTESIAN_POINT('Ctrl Pts',(-1.36714693221582,1.57928024643194,-1.268012642573));
#9862=CARTESIAN_POINT('Ctrl Pts',(-1.32510251806025,1.85175170782269,-0.821204880631625));
#9863=CARTESIAN_POINT('Ctrl Pts',(-1.30352961156712,1.94325916583521,-0.57194337379661));
#9864=CARTESIAN_POINT('Ctrl Pts',(-1.26217761857935,2.02455466379949,-0.0551650156779208));
#9865=CARTESIAN_POINT('Ctrl Pts',(-1.24316007249524,2.01468227469715,0.207169081980398));
#9866=CARTESIAN_POINT('Ctrl Pts',(-1.2011643193693,1.89474571919842,0.716511125263879));
#9867=CARTESIAN_POINT('Ctrl Pts',(-1.17957243215547,1.78467224709688,0.958334996833248));
#9868=CARTESIAN_POINT('Ctrl Pts',(-1.13816309807723,1.4794374337588,1.38311794236977));
#9869=CARTESIAN_POINT('Ctrl Pts',(-1.11918480959087,1.2882791099408,1.56271755609484));
#9870=CARTESIAN_POINT('Ctrl Pts',(-1.07723930261779,0.845185758698867,1.84097786631538));
#9871=CARTESIAN_POINT('Ctrl Pts',(-1.05562907829457,0.596805733715434,1.93581267466358));
#9872=CARTESIAN_POINT('Ctrl Pts',(-1.01416249047248,0.0812001570578579,
2.02362219580507));
#9873=CARTESIAN_POINT('Ctrl Pts',(-0.99521862998263,-0.180794988375118,
2.01716443761624));
#9874=CARTESIAN_POINT('Ctrl Pts',(-0.953324866943538,-0.691596166203094,
1.90402815017389));
#9875=CARTESIAN_POINT('Ctrl Pts',(-0.931697024099726,-0.93515080245912,
1.79697762511782));
#9876=CARTESIAN_POINT('Ctrl Pts',(-0.890173431001628,-1.36373603292118,
1.49725045325215));
#9877=CARTESIAN_POINT('Ctrl Pts',(-0.871258921075412,-1.54552869401676,
1.30876853444956));
#9878=CARTESIAN_POINT('Ctrl Pts',(-0.829418297971695,-1.8296663418148,0.869505805091247));
#9879=CARTESIAN_POINT('Ctrl Pts',(-0.807773623713855,-1.92788820551147,
0.622070168229358));
#9880=CARTESIAN_POINT('Ctrl Pts',(-0.766193433292469,-2.0223340702211,0.10770124781425));
#9881=CARTESIAN_POINT('Ctrl Pts',(-0.747302997047551,-2.0193398374198,-0.153950268255605));
#9882=CARTESIAN_POINT('Ctrl Pts',(-0.705516794228873,-1.9131155891858,-0.666182731595407));
#9883=CARTESIAN_POINT('Ctrl Pts',(-0.68385613666116,-1.80916028141189,-0.911456258058694));
#9884=CARTESIAN_POINT('Ctrl Pts',(-0.642219912899481,-1.51504612288649,
-1.34386574423529));
#9885=CARTESIAN_POINT('Ctrl Pts',(-0.623348126422726,-1.32926520574239,
-1.527872263121));
#9886=CARTESIAN_POINT('Ctrl Pts',(-0.583787298578959,-0.916549650383403,
-1.80283579070201));
#9887=CARTESIAN_POINT('Ctrl Pts',(-0.564384926046246,-0.697799062386865,
-1.89824973210959));
#9888=CARTESIAN_POINT('Ctrl Pts',(-0.532702841586254,-0.314104129907558,
-1.99007990973763));
#9889=CARTESIAN_POINT('Ctrl Pts',(-0.52034291965406,-0.157219629244434,
-2.008532));
#9890=CARTESIAN_POINT('Ctrl Pts',(-0.508531999999968,4.18345913466567E-13,
-2.008532));
#9891=CARTESIAN_POINT('Origin',(-2.93767550469109,0.,0.));
#9892=CARTESIAN_POINT('',(-3.19240120012393,-2.30940107675851,-4.));
#9893=CARTESIAN_POINT('',(-3.19240120012393,2.30940107675851,-4.));
#9894=CARTESIAN_POINT('Ctrl Pts',(-3.19240120011886,-2.30940107677608,-4.));
#9895=CARTESIAN_POINT('Ctrl Pts',(-3.8590678667944,2.22044604925031E-16,
-4.));
#9896=CARTESIAN_POINT('Ctrl Pts',(-3.19240120011886,2.30940107677608,-4.));
#9897=CARTESIAN_POINT('',(-3.19240120012393,-4.61880215351701,0.));
#9898=CARTESIAN_POINT('Ctrl Pts',(-3.19240120011885,-4.6188021535258,1.52242598350499E-11));
#9899=CARTESIAN_POINT('Ctrl Pts',(-3.8590678667944,-3.46410161513776,-2.));
#9900=CARTESIAN_POINT('Ctrl Pts',(-3.19240120011886,-2.30940107674972,-4.00000000001522));
#9901=CARTESIAN_POINT('',(-3.19240120012393,-2.30940107675851,4.));
#9902=CARTESIAN_POINT('Ctrl Pts',(-3.19240120011886,-2.30940107674972,4.00000000001521));
#9903=CARTESIAN_POINT('Ctrl Pts',(-3.8590678667944,-3.46410161513776,2.));
#9904=CARTESIAN_POINT('Ctrl Pts',(-3.19240120011886,-4.61880215352579,-1.52191983380731E-11));
#9905=CARTESIAN_POINT('',(-3.54966679003209,3.14368002532301E-16,4.));
#9906=CARTESIAN_POINT('Ctrl Pts',(-3.19240120011886,-2.30940107677608,4.));
#9907=CARTESIAN_POINT('Ctrl Pts',(-3.54966679003209,-1.07179676973155,4.));
#9908=CARTESIAN_POINT('Ctrl Pts',(-3.54966679003209,1.11859472472354E-15,
4.));
#9909=CARTESIAN_POINT('',(-4.,-3.94336269325448E-16,3.22));
#9910=CARTESIAN_POINT('',(-2.93767550469109,-6.19671280368561E-16,5.06));
#9911=CARTESIAN_POINT('Origin',(-4.,0.,0.));
#9912=CARTESIAN_POINT('',(-3.19240120012393,2.30940107675851,4.));
#9913=CARTESIAN_POINT('Ctrl Pts',(-3.54966679003209,1.11859472472354E-15,
4.));
#9914=CARTESIAN_POINT('Ctrl Pts',(-3.54966679003209,1.07179676973155,4.));
#9915=CARTESIAN_POINT('Ctrl Pts',(-3.19240120011886,2.30940107677607,4.));
#9916=CARTESIAN_POINT('',(-3.19240120012393,4.61880215351701,0.));
#9917=CARTESIAN_POINT('Ctrl Pts',(-3.19240120011885,4.6188021535258,-1.52242598350499E-11));
#9918=CARTESIAN_POINT('Ctrl Pts',(-3.8590678667944,3.46410161513776,2.));
#9919=CARTESIAN_POINT('Ctrl Pts',(-3.19240120011886,2.30940107674972,4.00000000001522));
#9920=CARTESIAN_POINT('Ctrl Pts',(-3.19240120011886,2.30940107674972,-4.00000000001521));
#9921=CARTESIAN_POINT('Ctrl Pts',(-3.8590678667944,3.46410161513776,-2.));
#9922=CARTESIAN_POINT('Ctrl Pts',(-3.19240120011886,4.61880215352579,1.52191983380731E-11));
#9923=CARTESIAN_POINT('Origin',(0.,0.,0.));
#9924=CARTESIAN_POINT('',(1.17539427474239E-16,0.663411757905302,-2.41037027020186));
#9925=CARTESIAN_POINT('Origin',(0.,0.,0.));
#9926=CARTESIAN_POINT('Ctrl Pts',(-1.82145964977565E-16,0.663411757905292,
-2.41037027020186));
#9927=CARTESIAN_POINT('Ctrl Pts',(-0.0068932752031904,0.499867287283901,
-2.44823338935451));
#9928=CARTESIAN_POINT('Ctrl Pts',(-0.0137115664211188,0.33294396450463,
-2.46959882520677));
#9929=CARTESIAN_POINT('Ctrl Pts',(-0.0270997986546331,-0.00565733357005639,
-2.47877910626091));
#9930=CARTESIAN_POINT('Ctrl Pts',(-0.0336564761924616,-0.177008197745316,
-2.46598363045078));
#9931=CARTESIAN_POINT('Ctrl Pts',(-0.0536637583285811,-0.659952657991195,
-2.37710123135134));
#9932=CARTESIAN_POINT('Ctrl Pts',(-0.0672921528648265,-0.959245802836347,
-2.25820164274285));
#9933=CARTESIAN_POINT('Ctrl Pts',(-0.0927875713568389,-1.46471243278332,
-1.93113485588623));
#9934=CARTESIAN_POINT('Ctrl Pts',(-0.105075936490514,-1.70142949321577,
-1.71908597546532));
#9935=CARTESIAN_POINT('Ctrl Pts',(-0.132290467527035,-2.07148587907461,
-1.18757222236683));
#9936=CARTESIAN_POINT('Ctrl Pts',(-0.145927106519498,-2.19635742991887,
-0.901652475941354));
#9937=CARTESIAN_POINT('Ctrl Pts',(-0.171531588164497,-2.32125889322368,
-0.330603170846493));
#9938=CARTESIAN_POINT('Ctrl Pts',(-0.183808945617099,-2.33860361927158,
-0.0247236227682734));
#9939=CARTESIAN_POINT('Ctrl Pts',(-0.210295427797897,-2.2342235021799,0.576950904578398));
#9940=CARTESIAN_POINT('Ctrl Pts',(-0.223339016646017,-2.13237831290703,
0.84734778897084));
#9941=CARTESIAN_POINT('Ctrl Pts',(-0.243011417696767,-1.90645192751628,
1.21693862929627));
#9942=CARTESIAN_POINT('Ctrl Pts',(-0.24962020758457,-1.81794099851076,1.33446859700807));
#9943=CARTESIAN_POINT('Ctrl Pts',(-0.262569893827658,-1.61882738726217,
1.55154278536559));
#9944=CARTESIAN_POINT('Ctrl Pts',(-0.268850102427555,-1.50744739092849,
1.65165556226842));
#9945=CARTESIAN_POINT('Ctrl Pts',(-0.28784942229089,-1.16344806195362,1.90152272333394));
#9946=CARTESIAN_POINT('Ctrl Pts',(-0.300818689630185,-0.911979820987807,
2.02001175976281));
#9947=CARTESIAN_POINT('Ctrl Pts',(-0.320467201912672,-0.508066949584239,
2.12420208011994));
#9948=CARTESIAN_POINT('Ctrl Pts',(-0.32709177611566,-0.367859794683295,
2.14621003927891));
#9949=CARTESIAN_POINT('Ctrl Pts',(-0.337013615803521,-0.151496210248655,
2.15897970641058));
#9950=CARTESIAN_POINT('Ctrl Pts',(-0.340430365784306,-0.0757839817297517,
2.15956963421569));
#9951=CARTESIAN_POINT('Ctrl Pts',(-0.343792495187436,2.27099480653155E-16,
2.15620750481256));
#9952=CARTESIAN_POINT('Origin',(-3.508532,0.,0.));
#9953=CARTESIAN_POINT('',(-4.,2.46710998658661,-0.40418846357189));
#9954=CARTESIAN_POINT('Origin',(-4.,0.,0.));
#9955=CARTESIAN_POINT('Ctrl Pts',(-3.50853200000446,-9.37083836906508E-11,
-2.00853200000446));
#9956=CARTESIAN_POINT('Ctrl Pts',(-3.51292702417713,-0.0922810368142426,
-2.01292702417282));
#9957=CARTESIAN_POINT('Ctrl Pts',(-3.51857752432441,-0.208898649734097,
-2.01229229041598));
#9958=CARTESIAN_POINT('Ctrl Pts',(-3.53087885357248,-0.454106642669512,
-1.9825908865936));
#9959=CARTESIAN_POINT('Ctrl Pts',(-3.53650469184044,-0.563552638557295,
-1.9601450116639));
#9960=CARTESIAN_POINT('Ctrl Pts',(-3.55356981611893,-0.887604345263331,
-1.86554842964995));
#9961=CARTESIAN_POINT('Ctrl Pts',(-3.56492765125652,-1.09259900510742,-1.76667555549241));
#9962=CARTESIAN_POINT('Ctrl Pts',(-3.58247411882797,-1.39111902687923,-1.55591193265632));
#9963=CARTESIAN_POINT('Ctrl Pts',(-3.58874370607916,-1.49596069762447,-1.46420141740028));
#9964=CARTESIAN_POINT('Ctrl Pts',(-3.60164700981519,-1.68459789727543,-1.26406206035305));
#9965=CARTESIAN_POINT('Ctrl Pts',(-3.60824813690499,-1.76884843111482,-1.15528455891842));
#9966=CARTESIAN_POINT('Ctrl Pts',(-3.62792724143012,-1.98494271219238,-0.812282569527967));
#9967=CARTESIAN_POINT('Ctrl Pts',(-3.64099804154009,-2.08364449732469,-0.560403869526387));
#9968=CARTESIAN_POINT('Ctrl Pts',(-3.66807436475461,-2.19066070805393,0.0121812493841459));
#9969=CARTESIAN_POINT('Ctrl Pts',(-3.68062554807944,-2.17463256315328,0.305991508728111));
#9970=CARTESIAN_POINT('Ctrl Pts',(-3.70581838685037,-2.06141327516712,0.832935131054126));
#9971=CARTESIAN_POINT('Ctrl Pts',(-3.71894428739146,-1.95164994292461,1.09195784432159));
#9972=CARTESIAN_POINT('Ctrl Pts',(-3.73813174295214,-1.71442518947555,1.44627404668417));
#9973=CARTESIAN_POINT('Ctrl Pts',(-3.74436525939159,-1.6207689605633,1.55946508773479));
#9974=CARTESIAN_POINT('Ctrl Pts',(-3.76368926437764,-1.30374829832282,1.87462298805652));
#9975=CARTESIAN_POINT('Ctrl Pts',(-3.77733071684782,-1.05165672040478,2.04203466813512));
#9976=CARTESIAN_POINT('Ctrl Pts',(-3.79751331327142,-0.637746828063753,
2.21215772464066));
#9977=CARTESIAN_POINT('Ctrl Pts',(-3.80410247062574,-0.495924536937652,
2.25493873023327));
#9978=CARTESIAN_POINT('Ctrl Pts',(-3.82519226905413,-0.0202166467251451,
2.34938256657904));
#9979=CARTESIAN_POINT('Ctrl Pts',(-3.83747842364639,0.289777401984434,2.33503990053325));
#9980=CARTESIAN_POINT('Ctrl Pts',(-3.86266234370501,0.857667212957973,2.2230575522556));
#9981=CARTESIAN_POINT('Ctrl Pts',(-3.87627217552642,1.1463214551877,2.10429183070078));
#9982=CARTESIAN_POINT('Ctrl Pts',(-3.90401447671096,1.69531375267038,1.73991032599821));
#9983=CARTESIAN_POINT('Ctrl Pts',(-3.91630521053648,1.91239288512789,1.50297344723526));
#9984=CARTESIAN_POINT('Ctrl Pts',(-3.94007316637035,2.22828134319281,1.03459998543546));
#9985=CARTESIAN_POINT('Ctrl Pts',(-3.95225872728684,2.34532113430431,0.771188063445417));
#9986=CARTESIAN_POINT('Ctrl Pts',(-3.97957344612241,2.50469052679756,0.127998548371377));
#9987=CARTESIAN_POINT('Ctrl Pts',(-3.9911790709379,2.49377286047805,-0.186882496097888));
#9988=CARTESIAN_POINT('Ctrl Pts',(-3.99999999999735,2.46710998659464,-0.404188463506497));
#9989=CARTESIAN_POINT('Origin',(0.,5.06,0.));
#9990=CARTESIAN_POINT('',(0.,4.61880215351701,0.));
#9991=CARTESIAN_POINT('',(0.,2.30940107675851,4.));
#9992=CARTESIAN_POINT('',(0.,4.61880215351701,0.));
#9993=CARTESIAN_POINT('',(0.,-2.30940107675851,4.));
#9994=CARTESIAN_POINT('',(0.,2.30940107675851,4.));
#9995=CARTESIAN_POINT('',(0.,-4.61880215351701,0.));
#9996=CARTESIAN_POINT('',(0.,-2.30940107675851,4.));
#9997=CARTESIAN_POINT('',(0.,-2.30940107675851,-4.));
#9998=CARTESIAN_POINT('',(0.,-4.61880215351701,0.));
#9999=CARTESIAN_POINT('',(0.,2.30940107675851,-4.));
#10000=CARTESIAN_POINT('',(0.,-2.30940107675851,-4.));
#10001=CARTESIAN_POINT('',(0.,2.30940107675851,-4.));
#10002=CARTESIAN_POINT('Origin',(0.000123745270384153,-0.0786025494032175,
-0.269984759888047));
#10003=CARTESIAN_POINT('Origin',(-4.52827338442856E-5,0.270013278081845,
0.0783217498640101));
#10004=CARTESIAN_POINT('Origin',(-4.,0.,0.));
#10005=CARTESIAN_POINT('Origin',(-3.99996492800005,-0.0784507930919776,
-0.270006358878946));
#10006=CARTESIAN_POINT('Origin',(-4.00005184704125,0.270010503487591,0.0783328141479592));
#10007=CARTESIAN_POINT('Origin',(-4.,4.61880215351701,0.));
#10008=CARTESIAN_POINT('',(-4.,2.30940107675851,4.));
#10009=CARTESIAN_POINT('',(-4.,4.61880215351701,0.));
#10010=CARTESIAN_POINT('Origin',(-4.,2.30940107675851,-4.));
#10011=CARTESIAN_POINT('',(-4.,2.30940107675851,-4.));
#10012=CARTESIAN_POINT('Origin',(-4.,-2.30940107675851,-4.));
#10013=CARTESIAN_POINT('',(-4.,-2.30940107675851,-4.));
#10014=CARTESIAN_POINT('Origin',(-4.,-4.61880215351701,0.));
#10015=CARTESIAN_POINT('',(-4.,-4.61880215351701,0.));
#10016=CARTESIAN_POINT('Origin',(-4.,-2.30940107675851,4.));
#10017=CARTESIAN_POINT('',(-4.,-2.30940107675851,4.));
#10018=CARTESIAN_POINT('Origin',(-4.,2.30940107675851,4.));
#10019=CARTESIAN_POINT('Origin',(-4.1335320013656,6.79957634403871E-15,
-6.66133814775094E-15));
#10020=CARTESIAN_POINT('Ctrl Pts',(-3.57103200136559,3.12260180609148E-16,
2.549797875));
#10021=CARTESIAN_POINT('Ctrl Pts',(-3.50853200136559,-1.0561608611351,2.549797875));
#10022=CARTESIAN_POINT('Ctrl Pts',(-3.4460320013656,-1.80297936806755,1.80297936806755));
#10023=CARTESIAN_POINT('Ctrl Pts',(-3.3835320013656,-2.549797875,1.0561608611351));
#10024=CARTESIAN_POINT('Ctrl Pts',(-3.3210320013656,-2.549797875,4.68390270913721E-16));
#10025=CARTESIAN_POINT('Ctrl Pts',(-3.2585320013656,-2.549797875,-1.0561608611351));
#10026=CARTESIAN_POINT('Ctrl Pts',(-3.1960320013656,-1.80297936806755,-1.80297936806755));
#10027=CARTESIAN_POINT('Ctrl Pts',(-3.13353200136559,-1.0561608611351,-2.549797875));
#10028=CARTESIAN_POINT('Ctrl Pts',(-3.07103200136559,0.,-2.549797875));
#10029=CARTESIAN_POINT('Ctrl Pts',(-3.00853200136559,1.0561608611351,-2.549797875));
#10030=CARTESIAN_POINT('Ctrl Pts',(-2.94603200136559,1.80297936806755,-1.80297936806755));
#10031=CARTESIAN_POINT('Ctrl Pts',(-2.88353200136559,2.549797875,-1.0561608611351));
#10032=CARTESIAN_POINT('Ctrl Pts',(-2.82103200136559,2.549797875,-1.56130090304574E-16));
#10033=CARTESIAN_POINT('Ctrl Pts',(-2.75853200136559,2.549797875,1.0561608611351));
#10034=CARTESIAN_POINT('Ctrl Pts',(-2.6960320013656,1.80297936806755,1.80297936806755));
#10035=CARTESIAN_POINT('Ctrl Pts',(-2.6335320013656,1.0561608611351,2.549797875));
#10036=CARTESIAN_POINT('Ctrl Pts',(-2.5710320013656,3.12260180609148E-16,
2.549797875));
#10037=CARTESIAN_POINT('Ctrl Pts',(-3.6960320013656,3.12260180609148E-16,
2.549797875));
#10038=CARTESIAN_POINT('Ctrl Pts',(-3.63353200136559,-1.0561608611351,2.549797875));
#10039=CARTESIAN_POINT('Ctrl Pts',(-3.57103200136559,-1.80297936806755,
1.80297936806755));
#10040=CARTESIAN_POINT('Ctrl Pts',(-3.50853200136559,-2.549797875,1.0561608611351));
#10041=CARTESIAN_POINT('Ctrl Pts',(-3.4460320013656,-2.549797875,4.68390270913721E-16));
#10042=CARTESIAN_POINT('Ctrl Pts',(-3.3835320013656,-2.549797875,-1.0561608611351));
#10043=CARTESIAN_POINT('Ctrl Pts',(-3.3210320013656,-1.80297936806755,-1.80297936806755));
#10044=CARTESIAN_POINT('Ctrl Pts',(-3.2585320013656,-1.0561608611351,-2.549797875));
#10045=CARTESIAN_POINT('Ctrl Pts',(-3.1960320013656,0.,-2.549797875));
#10046=CARTESIAN_POINT('Ctrl Pts',(-3.13353200136559,1.0561608611351,-2.549797875));
#10047=CARTESIAN_POINT('Ctrl Pts',(-3.07103200136559,1.80297936806755,-1.80297936806755));
#10048=CARTESIAN_POINT('Ctrl Pts',(-3.00853200136559,2.549797875,-1.0561608611351));
#10049=CARTESIAN_POINT('Ctrl Pts',(-2.94603200136559,2.549797875,-1.56130090304574E-16));
#10050=CARTESIAN_POINT('Ctrl Pts',(-2.88353200136559,2.549797875,1.0561608611351));
#10051=CARTESIAN_POINT('Ctrl Pts',(-2.82103200136559,1.80297936806755,1.80297936806755));
#10052=CARTESIAN_POINT('Ctrl Pts',(-2.75853200136559,1.0561608611351,2.549797875));
#10053=CARTESIAN_POINT('Ctrl Pts',(-2.6960320013656,3.12260180609148E-16,
2.549797875));
#10054=CARTESIAN_POINT('Ctrl Pts',(-4.50855844600304,0.,-2.00848619417908));
#10055=CARTESIAN_POINT('Ctrl Pts',(-4.44605844600304,0.831942221468096,
-2.00848619417908));
#10056=CARTESIAN_POINT('Ctrl Pts',(-4.38355844600304,1.42021420782359,-1.42021420782359));
#10057=CARTESIAN_POINT('Ctrl Pts',(-4.32105844600304,2.00848619417908,-0.831942221468096));
#10058=CARTESIAN_POINT('Ctrl Pts',(-4.25855844600304,2.00848619417908,-1.22984309441653E-16));
#10059=CARTESIAN_POINT('Ctrl Pts',(-4.19605844600304,2.00848619417908,0.831942221468096));
#10060=CARTESIAN_POINT('Ctrl Pts',(-4.13355844600304,1.42021420782359,1.42021420782359));
#10061=CARTESIAN_POINT('Ctrl Pts',(-4.07105844600304,0.831942221468096,
2.00848619417908));
#10062=CARTESIAN_POINT('Ctrl Pts',(-4.00855844600304,2.45968618883306E-16,
2.00848619417908));
#10063=CARTESIAN_POINT('Ctrl Pts',(-3.94605844600304,-0.831942221468095,
2.00848619417908));
#10064=CARTESIAN_POINT('Ctrl Pts',(-3.88355844600304,-1.42021420782359,
1.42021420782359));
#10065=CARTESIAN_POINT('Ctrl Pts',(-3.82105844600304,-2.00848619417908,
0.831942221468097));
#10066=CARTESIAN_POINT('Ctrl Pts',(-3.75855844600304,-2.00848619417908,
3.68952928324959E-16));
#10067=CARTESIAN_POINT('Ctrl Pts',(-3.69605844600304,-2.00848619417908,
-0.831942221468096));
#10068=CARTESIAN_POINT('Ctrl Pts',(-3.63355844600304,-1.42021420782359,
-1.42021420782359));
#10069=CARTESIAN_POINT('Ctrl Pts',(-3.57105844600304,-0.831942221468097,
-2.00848619417908));
#10070=CARTESIAN_POINT('Ctrl Pts',(-3.50855844600304,0.,-2.00848619417908));
#10071=CARTESIAN_POINT('Ctrl Pts',(-3.44605844600304,0.831942221468096,
-2.00848619417908));
#10072=CARTESIAN_POINT('Ctrl Pts',(-3.38355844600304,1.42021420782359,-1.42021420782359));
#10073=CARTESIAN_POINT('Ctrl Pts',(-3.32105844600304,2.00848619417908,-0.831942221468096));
#10074=CARTESIAN_POINT('Ctrl Pts',(-3.25855844600304,2.00848619417908,-1.22984309441653E-16));
#10075=CARTESIAN_POINT('Ctrl Pts',(-3.19605844600304,2.00848619417908,0.831942221468096));
#10076=CARTESIAN_POINT('Ctrl Pts',(-3.13355844600304,1.42021420782359,1.42021420782359));
#10077=CARTESIAN_POINT('Ctrl Pts',(-3.07105844600304,0.831942221468096,
2.00848619417908));
#10078=CARTESIAN_POINT('Ctrl Pts',(-3.00855844600304,2.45968618883306E-16,
2.00848619417908));
#10079=CARTESIAN_POINT('Ctrl Pts',(-2.94605844600304,-0.831942221468095,
2.00848619417908));
#10080=CARTESIAN_POINT('Ctrl Pts',(-2.88355844600304,-1.42021420782359,
1.42021420782359));
#10081=CARTESIAN_POINT('Ctrl Pts',(-2.82105844600304,-2.00848619417908,
0.831942221468097));
#10082=CARTESIAN_POINT('Ctrl Pts',(-2.75855844600304,-2.00848619417908,
3.68952928324959E-16));
#10083=CARTESIAN_POINT('Ctrl Pts',(-2.69605844600304,-2.00848619417908,
-0.831942221468096));
#10084=CARTESIAN_POINT('Ctrl Pts',(-2.63355844600304,-1.42021420782359,
-1.42021420782359));
#10085=CARTESIAN_POINT('Ctrl Pts',(-2.57105844600304,-0.831942221468097,
-2.00848619417908));
#10086=CARTESIAN_POINT('Ctrl Pts',(-2.50855844600304,0.,-2.00848619417908));
#10087=CARTESIAN_POINT('Ctrl Pts',(-2.44605844600304,0.831942221468096,
-2.00848619417908));
#10088=CARTESIAN_POINT('Ctrl Pts',(-2.38355844600304,1.42021420782359,-1.42021420782359));
#10089=CARTESIAN_POINT('Ctrl Pts',(-2.32105844600304,2.00848619417908,-0.831942221468096));
#10090=CARTESIAN_POINT('Ctrl Pts',(-2.25855844600304,2.00848619417908,-1.22984309441653E-16));
#10091=CARTESIAN_POINT('Ctrl Pts',(-2.19605844600304,2.00848619417908,0.831942221468096));
#10092=CARTESIAN_POINT('Ctrl Pts',(-2.13355844600304,1.42021420782359,1.42021420782359));
#10093=CARTESIAN_POINT('Ctrl Pts',(-2.07105844600304,0.831942221468096,
2.00848619417908));
#10094=CARTESIAN_POINT('Ctrl Pts',(-2.00855844600304,2.45968618883306E-16,
2.00848619417908));
#10095=CARTESIAN_POINT('Ctrl Pts',(-1.94605844600304,-0.831942221468095,
2.00848619417908));
#10096=CARTESIAN_POINT('Ctrl Pts',(-1.88355844600304,-1.42021420782359,
1.42021420782359));
#10097=CARTESIAN_POINT('Ctrl Pts',(-1.82105844600304,-2.00848619417908,
0.831942221468097));
#10098=CARTESIAN_POINT('Ctrl Pts',(-1.75855844600304,-2.00848619417908,
3.68952928324959E-16));
#10099=CARTESIAN_POINT('Ctrl Pts',(-1.69605844600304,-2.00848619417908,
-0.831942221468096));
#10100=CARTESIAN_POINT('Ctrl Pts',(-1.63355844600304,-1.42021420782359,
-1.42021420782359));
#10101=CARTESIAN_POINT('Ctrl Pts',(-1.57105844600304,-0.831942221468097,
-2.00848619417908));
#10102=CARTESIAN_POINT('Ctrl Pts',(-1.50855844600304,0.,-2.00848619417908));
#10103=CARTESIAN_POINT('Ctrl Pts',(-1.44605844600304,0.831942221468096,
-2.00848619417908));
#10104=CARTESIAN_POINT('Ctrl Pts',(-1.38355844600304,1.42021420782359,-1.42021420782359));
#10105=CARTESIAN_POINT('Ctrl Pts',(-1.32105844600304,2.00848619417908,-0.831942221468096));
#10106=CARTESIAN_POINT('Ctrl Pts',(-1.25855844600304,2.00848619417908,-1.22984309441653E-16));
#10107=CARTESIAN_POINT('Ctrl Pts',(-1.19605844600304,2.00848619417908,0.831942221468096));
#10108=CARTESIAN_POINT('Ctrl Pts',(-1.13355844600304,1.42021420782359,1.42021420782359));
#10109=CARTESIAN_POINT('Ctrl Pts',(-1.07105844600304,0.831942221468096,
2.00848619417908));
#10110=CARTESIAN_POINT('Ctrl Pts',(-1.00855844600304,2.45968618883306E-16,
2.00848619417908));
#10111=CARTESIAN_POINT('Ctrl Pts',(-0.94605844600304,-0.831942221468095,
2.00848619417908));
#10112=CARTESIAN_POINT('Ctrl Pts',(-0.88355844600304,-1.42021420782359,
1.42021420782359));
#10113=CARTESIAN_POINT('Ctrl Pts',(-0.82105844600304,-2.00848619417908,
0.831942221468097));
#10114=CARTESIAN_POINT('Ctrl Pts',(-0.75855844600304,-2.00848619417908,
3.68952928324959E-16));
#10115=CARTESIAN_POINT('Ctrl Pts',(-0.696058446003041,-2.00848619417908,
-0.831942221468096));
#10116=CARTESIAN_POINT('Ctrl Pts',(-0.63355844600304,-1.42021420782359,
-1.42021420782359));
#10117=CARTESIAN_POINT('Ctrl Pts',(-0.571058446003041,-0.831942221468097,
-2.00848619417908));
#10118=CARTESIAN_POINT('Ctrl Pts',(-0.50855844600304,0.,-2.00848619417908));
#10119=CARTESIAN_POINT('Ctrl Pts',(-0.446058446003041,0.831942221468096,
-2.00848619417908));
#10120=CARTESIAN_POINT('Ctrl Pts',(-0.38355844600304,1.42021420782359,-1.42021420782359));
#10121=CARTESIAN_POINT('Ctrl Pts',(-0.321058446003041,2.00848619417908,
-0.831942221468096));
#10122=CARTESIAN_POINT('Ctrl Pts',(-0.25855844600304,2.00848619417908,-1.22984309441653E-16));
#10123=CARTESIAN_POINT('Ctrl Pts',(-0.19605844600304,2.00848619417908,0.831942221468096));
#10124=CARTESIAN_POINT('Ctrl Pts',(-0.13355844600304,1.42021420782359,1.42021420782359));
#10125=CARTESIAN_POINT('Ctrl Pts',(-0.0710584460030402,0.831942221468096,
2.00848619417908));
#10126=CARTESIAN_POINT('Ctrl Pts',(-0.00855844600304013,2.45968618883306E-16,
2.00848619417908));
#10127=CARTESIAN_POINT('Ctrl Pts',(0.0539415539969591,-0.831942221468095,
2.00848619417908));
#10128=CARTESIAN_POINT('Ctrl Pts',(0.11644155399696,-1.42021420782359,1.42021420782359));
#10129=CARTESIAN_POINT('Ctrl Pts',(0.178941553996959,-2.00848619417908,
0.831942221468097));
#10130=CARTESIAN_POINT('Ctrl Pts',(0.24144155399696,-2.00848619417908,3.68952928324959E-16));
#10131=CARTESIAN_POINT('Ctrl Pts',(0.303941553996959,-2.00848619417908,
-0.831942221468096));
#10132=CARTESIAN_POINT('Ctrl Pts',(0.36644155399696,-1.42021420782359,-1.42021420782359));
#10133=CARTESIAN_POINT('Ctrl Pts',(0.428941553996959,-0.831942221468097,
-2.00848619417908));
#10134=CARTESIAN_POINT('Ctrl Pts',(0.49144155399696,0.,-2.00848619417908));
#10135=CARTESIAN_POINT('Ctrl Pts',(-4.19603200136559,0.,-2.549797875));
#10136=CARTESIAN_POINT('Ctrl Pts',(-4.13353200136559,1.0561608611351,-2.549797875));
#10137=CARTESIAN_POINT('Ctrl Pts',(-4.07103200136559,1.80297936806755,-1.80297936806755));
#10138=CARTESIAN_POINT('Ctrl Pts',(-4.00853200136559,2.549797875,-1.0561608611351));
#10139=CARTESIAN_POINT('Ctrl Pts',(-3.9460320013656,2.549797875,-1.56130090304574E-16));
#10140=CARTESIAN_POINT('Ctrl Pts',(-3.88353200136559,2.549797875,1.0561608611351));
#10141=CARTESIAN_POINT('Ctrl Pts',(-3.8210320013656,1.80297936806755,1.80297936806755));
#10142=CARTESIAN_POINT('Ctrl Pts',(-3.75853200136559,1.0561608611351,2.549797875));
#10143=CARTESIAN_POINT('Ctrl Pts',(-3.6960320013656,3.12260180609148E-16,
2.549797875));
#10144=CARTESIAN_POINT('Ctrl Pts',(-3.63353200136559,-1.0561608611351,2.549797875));
#10145=CARTESIAN_POINT('Ctrl Pts',(-3.57103200136559,-1.80297936806755,
1.80297936806755));
#10146=CARTESIAN_POINT('Ctrl Pts',(-3.50853200136559,-2.549797875,1.0561608611351));
#10147=CARTESIAN_POINT('Ctrl Pts',(-3.4460320013656,-2.549797875,4.68390270913721E-16));
#10148=CARTESIAN_POINT('Ctrl Pts',(-3.3835320013656,-2.549797875,-1.0561608611351));
#10149=CARTESIAN_POINT('Ctrl Pts',(-3.3210320013656,-1.80297936806755,-1.80297936806755));
#10150=CARTESIAN_POINT('Ctrl Pts',(-3.2585320013656,-1.0561608611351,-2.549797875));
#10151=CARTESIAN_POINT('Ctrl Pts',(-3.1960320013656,0.,-2.549797875));
#10152=CARTESIAN_POINT('Ctrl Pts',(-3.13353200136559,1.0561608611351,-2.549797875));
#10153=CARTESIAN_POINT('Ctrl Pts',(-3.07103200136559,1.80297936806755,-1.80297936806755));
#10154=CARTESIAN_POINT('Ctrl Pts',(-3.00853200136559,2.549797875,-1.0561608611351));
#10155=CARTESIAN_POINT('Ctrl Pts',(-2.94603200136559,2.549797875,-1.56130090304574E-16));
#10156=CARTESIAN_POINT('Ctrl Pts',(-2.88353200136559,2.549797875,1.0561608611351));
#10157=CARTESIAN_POINT('Ctrl Pts',(-2.82103200136559,1.80297936806755,1.80297936806755));
#10158=CARTESIAN_POINT('Ctrl Pts',(-2.75853200136559,1.0561608611351,2.549797875));
#10159=CARTESIAN_POINT('Ctrl Pts',(-2.6960320013656,3.12260180609148E-16,
2.549797875));
#10160=CARTESIAN_POINT('Ctrl Pts',(-2.63353200136559,-1.0561608611351,2.549797875));
#10161=CARTESIAN_POINT('Ctrl Pts',(-2.5710320013656,-1.80297936806755,1.80297936806755));
#10162=CARTESIAN_POINT('Ctrl Pts',(-2.5085320013656,-2.549797875,1.0561608611351));
#10163=CARTESIAN_POINT('Ctrl Pts',(-2.44603200136559,-2.549797875,4.68390270913721E-16));
#10164=CARTESIAN_POINT('Ctrl Pts',(-2.38353200136559,-2.549797875,-1.0561608611351));
#10165=CARTESIAN_POINT('Ctrl Pts',(-2.3210320013656,-1.80297936806755,-1.80297936806755));
#10166=CARTESIAN_POINT('Ctrl Pts',(-2.25853200136559,-1.0561608611351,-2.549797875));
#10167=CARTESIAN_POINT('Ctrl Pts',(-2.1960320013656,0.,-2.549797875));
#10168=CARTESIAN_POINT('Ctrl Pts',(-2.13353200136559,1.0561608611351,-2.549797875));
#10169=CARTESIAN_POINT('Ctrl Pts',(-2.07103200136559,1.80297936806755,-1.80297936806755));
#10170=CARTESIAN_POINT('Ctrl Pts',(-2.00853200136559,2.549797875,-1.0561608611351));
#10171=CARTESIAN_POINT('Ctrl Pts',(-1.9460320013656,2.549797875,-1.56130090304574E-16));
#10172=CARTESIAN_POINT('Ctrl Pts',(-1.8835320013656,2.549797875,1.0561608611351));
#10173=CARTESIAN_POINT('Ctrl Pts',(-1.82103200136559,1.80297936806755,1.80297936806755));
#10174=CARTESIAN_POINT('Ctrl Pts',(-1.7585320013656,1.0561608611351,2.549797875));
#10175=CARTESIAN_POINT('Ctrl Pts',(-1.69603200136559,3.12260180609148E-16,
2.549797875));
#10176=CARTESIAN_POINT('Ctrl Pts',(-1.63353200136559,-1.0561608611351,2.549797875));
#10177=CARTESIAN_POINT('Ctrl Pts',(-1.5710320013656,-1.80297936806755,1.80297936806755));
#10178=CARTESIAN_POINT('Ctrl Pts',(-1.50853200136559,-2.549797875,1.0561608611351));
#10179=CARTESIAN_POINT('Ctrl Pts',(-1.44603200136559,-2.549797875,4.68390270913721E-16));
#10180=CARTESIAN_POINT('Ctrl Pts',(-1.38353200136559,-2.549797875,-1.0561608611351));
#10181=CARTESIAN_POINT('Ctrl Pts',(-1.32103200136559,-1.80297936806755,
-1.80297936806755));
#10182=CARTESIAN_POINT('Ctrl Pts',(-1.25853200136559,-1.0561608611351,-2.549797875));
#10183=CARTESIAN_POINT('Ctrl Pts',(-1.19603200136559,0.,-2.549797875));
#10184=CARTESIAN_POINT('Ctrl Pts',(-1.13353200136559,1.0561608611351,-2.549797875));
#10185=CARTESIAN_POINT('Ctrl Pts',(-1.07103200136559,1.80297936806755,-1.80297936806755));
#10186=CARTESIAN_POINT('Ctrl Pts',(-1.00853200136559,2.549797875,-1.0561608611351));
#10187=CARTESIAN_POINT('Ctrl Pts',(-0.946032001365594,2.549797875,-1.56130090304574E-16));
#10188=CARTESIAN_POINT('Ctrl Pts',(-0.883532001365594,2.549797875,1.0561608611351));
#10189=CARTESIAN_POINT('Ctrl Pts',(-0.821032001365594,1.80297936806755,
1.80297936806755));
#10190=CARTESIAN_POINT('Ctrl Pts',(-0.758532001365594,1.0561608611351,2.549797875));
#10191=CARTESIAN_POINT('Ctrl Pts',(-0.696032001365594,3.12260180609148E-16,
2.549797875));
#10192=CARTESIAN_POINT('Ctrl Pts',(-0.633532001365594,-1.0561608611351,
2.549797875));
#10193=CARTESIAN_POINT('Ctrl Pts',(-0.571032001365594,-1.80297936806755,
1.80297936806755));
#10194=CARTESIAN_POINT('Ctrl Pts',(-0.508532001365594,-2.549797875,1.0561608611351));
#10195=CARTESIAN_POINT('Ctrl Pts',(-0.446032001365594,-2.549797875,4.68390270913721E-16));
#10196=CARTESIAN_POINT('Ctrl Pts',(-0.383532001365594,-2.549797875,-1.0561608611351));
#10197=CARTESIAN_POINT('Ctrl Pts',(-0.321032001365594,-1.80297936806755,
-1.80297936806755));
#10198=CARTESIAN_POINT('Ctrl Pts',(-0.258532001365594,-1.0561608611351,
-2.549797875));
#10199=CARTESIAN_POINT('Ctrl Pts',(-0.196032001365594,0.,-2.549797875));
#10200=CARTESIAN_POINT('Ctrl Pts',(-0.133532001365594,1.0561608611351,-2.549797875));
#10201=CARTESIAN_POINT('Ctrl Pts',(-0.0710320013655938,1.80297936806755,
-1.80297936806755));
#10202=CARTESIAN_POINT('Ctrl Pts',(-0.00853200136559373,2.549797875,-1.0561608611351));
#10203=CARTESIAN_POINT('Ctrl Pts',(0.0539679986344063,2.549797875,-1.56130090304574E-16));
#10204=CARTESIAN_POINT('Ctrl Pts',(0.116467998634406,2.549797875,1.0561608611351));
#10205=CARTESIAN_POINT('Ctrl Pts',(0.178967998634407,1.80297936806755,1.80297936806755));
#10206=CARTESIAN_POINT('Ctrl Pts',(0.241467998634406,1.0561608611351,2.549797875));
#10207=CARTESIAN_POINT('Ctrl Pts',(0.303967998634406,3.12260180609148E-16,
2.549797875));
#10208=CARTESIAN_POINT('Ctrl Pts',(0.366467998634406,-1.0561608611351,2.549797875));
#10209=CARTESIAN_POINT('Ctrl Pts',(0.428967998634406,-1.80297936806755,
1.80297936806755));
#10210=CARTESIAN_POINT('Ctrl Pts',(0.491467998634406,-2.549797875,1.0561608611351));
#10211=CARTESIAN_POINT('Ctrl Pts',(0.553967998634406,-2.549797875,4.68390270913721E-16));
#10212=CARTESIAN_POINT('Ctrl Pts',(0.616467998634407,-2.549797875,-1.0561608611351));
#10213=CARTESIAN_POINT('Ctrl Pts',(0.678967998634406,-1.80297936806755,
-1.80297936806755));
#10214=CARTESIAN_POINT('Ctrl Pts',(0.741467998634407,-1.0561608611351,-2.549797875));
#10215=CARTESIAN_POINT('Ctrl Pts',(0.803967998634406,0.,-2.549797875));
#10216=CARTESIAN_POINT('Ctrl Pts',(-4.07103200136559,0.,-2.549797875));
#10217=CARTESIAN_POINT('Ctrl Pts',(-4.00853200136559,1.0561608611351,-2.549797875));
#10218=CARTESIAN_POINT('Ctrl Pts',(-3.9460320013656,1.80297936806755,-1.80297936806755));
#10219=CARTESIAN_POINT('Ctrl Pts',(-3.88353200136559,2.549797875,-1.0561608611351));
#10220=CARTESIAN_POINT('Ctrl Pts',(-3.8210320013656,2.549797875,-1.56130090304574E-16));
#10221=CARTESIAN_POINT('Ctrl Pts',(-3.75853200136559,2.549797875,1.0561608611351));
#10222=CARTESIAN_POINT('Ctrl Pts',(-3.6960320013656,1.80297936806755,1.80297936806755));
#10223=CARTESIAN_POINT('Ctrl Pts',(-3.63353200136559,1.0561608611351,2.549797875));
#10224=CARTESIAN_POINT('Ctrl Pts',(-3.57103200136559,3.12260180609148E-16,
2.549797875));
#10225=CARTESIAN_POINT('Ctrl Pts',(-3.50853200136559,-1.0561608611351,2.549797875));
#10226=CARTESIAN_POINT('Ctrl Pts',(-3.4460320013656,-1.80297936806755,1.80297936806755));
#10227=CARTESIAN_POINT('Ctrl Pts',(-3.3835320013656,-2.549797875,1.0561608611351));
#10228=CARTESIAN_POINT('Ctrl Pts',(-3.3210320013656,-2.549797875,4.68390270913721E-16));
#10229=CARTESIAN_POINT('Ctrl Pts',(-3.2585320013656,-2.549797875,-1.0561608611351));
#10230=CARTESIAN_POINT('Ctrl Pts',(-3.1960320013656,-1.80297936806755,-1.80297936806755));
#10231=CARTESIAN_POINT('Ctrl Pts',(-3.13353200136559,-1.0561608611351,-2.549797875));
#10232=CARTESIAN_POINT('Ctrl Pts',(-3.07103200136559,0.,-2.549797875));
#10233=CARTESIAN_POINT('Ctrl Pts',(-3.00853200136559,1.0561608611351,-2.549797875));
#10234=CARTESIAN_POINT('Ctrl Pts',(-2.94603200136559,1.80297936806755,-1.80297936806755));
#10235=CARTESIAN_POINT('Ctrl Pts',(-2.88353200136559,2.549797875,-1.0561608611351));
#10236=CARTESIAN_POINT('Ctrl Pts',(-2.82103200136559,2.549797875,-1.56130090304574E-16));
#10237=CARTESIAN_POINT('Ctrl Pts',(-2.75853200136559,2.549797875,1.0561608611351));
#10238=CARTESIAN_POINT('Ctrl Pts',(-2.6960320013656,1.80297936806755,1.80297936806755));
#10239=CARTESIAN_POINT('Ctrl Pts',(-2.63353200136559,1.0561608611351,2.549797875));
#10240=CARTESIAN_POINT('Ctrl Pts',(-2.5710320013656,3.12260180609148E-16,
2.549797875));
#10241=CARTESIAN_POINT('Ctrl Pts',(-2.5085320013656,-1.0561608611351,2.549797875));
#10242=CARTESIAN_POINT('Ctrl Pts',(-2.44603200136559,-1.80297936806755,
1.80297936806755));
#10243=CARTESIAN_POINT('Ctrl Pts',(-2.38353200136559,-2.549797875,1.0561608611351));
#10244=CARTESIAN_POINT('Ctrl Pts',(-2.3210320013656,-2.549797875,4.68390270913721E-16));
#10245=CARTESIAN_POINT('Ctrl Pts',(-2.25853200136559,-2.549797875,-1.0561608611351));
#10246=CARTESIAN_POINT('Ctrl Pts',(-2.1960320013656,-1.80297936806755,-1.80297936806755));
#10247=CARTESIAN_POINT('Ctrl Pts',(-2.13353200136559,-1.0561608611351,-2.549797875));
#10248=CARTESIAN_POINT('Ctrl Pts',(-2.07103200136559,0.,-2.549797875));
#10249=CARTESIAN_POINT('Ctrl Pts',(-2.00853200136559,1.0561608611351,-2.549797875));
#10250=CARTESIAN_POINT('Ctrl Pts',(-1.9460320013656,1.80297936806755,-1.80297936806755));
#10251=CARTESIAN_POINT('Ctrl Pts',(-1.8835320013656,2.549797875,-1.0561608611351));
#10252=CARTESIAN_POINT('Ctrl Pts',(-1.82103200136559,2.549797875,-1.56130090304574E-16));
#10253=CARTESIAN_POINT('Ctrl Pts',(-1.7585320013656,2.549797875,1.0561608611351));
#10254=CARTESIAN_POINT('Ctrl Pts',(-1.69603200136559,1.80297936806755,1.80297936806755));
#10255=CARTESIAN_POINT('Ctrl Pts',(-1.63353200136559,1.0561608611351,2.549797875));
#10256=CARTESIAN_POINT('Ctrl Pts',(-1.5710320013656,3.12260180609148E-16,
2.549797875));
#10257=CARTESIAN_POINT('Ctrl Pts',(-1.50853200136559,-1.0561608611351,2.549797875));
#10258=CARTESIAN_POINT('Ctrl Pts',(-1.44603200136559,-1.80297936806755,
1.80297936806755));
#10259=CARTESIAN_POINT('Ctrl Pts',(-1.38353200136559,-2.549797875,1.0561608611351));
#10260=CARTESIAN_POINT('Ctrl Pts',(-1.32103200136559,-2.549797875,4.68390270913721E-16));
#10261=CARTESIAN_POINT('Ctrl Pts',(-1.25853200136559,-2.549797875,-1.0561608611351));
#10262=CARTESIAN_POINT('Ctrl Pts',(-1.19603200136559,-1.80297936806755,
-1.80297936806755));
#10263=CARTESIAN_POINT('Ctrl Pts',(-1.13353200136559,-1.0561608611351,-2.549797875));
#10264=CARTESIAN_POINT('Ctrl Pts',(-1.07103200136559,0.,-2.549797875));
#10265=CARTESIAN_POINT('Ctrl Pts',(-1.00853200136559,1.0561608611351,-2.549797875));
#10266=CARTESIAN_POINT('Ctrl Pts',(-0.946032001365594,1.80297936806755,
-1.80297936806755));
#10267=CARTESIAN_POINT('Ctrl Pts',(-0.883532001365593,2.549797875,-1.0561608611351));
#10268=CARTESIAN_POINT('Ctrl Pts',(-0.821032001365594,2.549797875,-1.56130090304574E-16));
#10269=CARTESIAN_POINT('Ctrl Pts',(-0.758532001365594,2.549797875,1.0561608611351));
#10270=CARTESIAN_POINT('Ctrl Pts',(-0.696032001365594,1.80297936806755,
1.80297936806755));
#10271=CARTESIAN_POINT('Ctrl Pts',(-0.633532001365594,1.0561608611351,2.549797875));
#10272=CARTESIAN_POINT('Ctrl Pts',(-0.571032001365594,3.12260180609148E-16,
2.549797875));
#10273=CARTESIAN_POINT('Ctrl Pts',(-0.508532001365594,-1.0561608611351,
2.549797875));
#10274=CARTESIAN_POINT('Ctrl Pts',(-0.446032001365594,-1.80297936806755,
1.80297936806755));
#10275=CARTESIAN_POINT('Ctrl Pts',(-0.383532001365594,-2.549797875,1.0561608611351));
#10276=CARTESIAN_POINT('Ctrl Pts',(-0.321032001365594,-2.549797875,4.68390270913721E-16));
#10277=CARTESIAN_POINT('Ctrl Pts',(-0.258532001365594,-2.549797875,-1.0561608611351));
#10278=CARTESIAN_POINT('Ctrl Pts',(-0.196032001365594,-1.80297936806755,
-1.80297936806755));
#10279=CARTESIAN_POINT('Ctrl Pts',(-0.133532001365594,-1.0561608611351,
-2.549797875));
#10280=CARTESIAN_POINT('Ctrl Pts',(-0.0710320013655938,0.,-2.549797875));
#10281=CARTESIAN_POINT('Ctrl Pts',(-0.00853200136559373,1.0561608611351,
-2.549797875));
#10282=CARTESIAN_POINT('Ctrl Pts',(0.0539679986344063,1.80297936806755,
-1.80297936806755));
#10283=CARTESIAN_POINT('Ctrl Pts',(0.116467998634406,2.549797875,-1.0561608611351));
#10284=CARTESIAN_POINT('Ctrl Pts',(0.178967998634407,2.549797875,-1.56130090304574E-16));
#10285=CARTESIAN_POINT('Ctrl Pts',(0.241467998634406,2.549797875,1.0561608611351));
#10286=CARTESIAN_POINT('Ctrl Pts',(0.303967998634406,1.80297936806755,1.80297936806755));
#10287=CARTESIAN_POINT('Ctrl Pts',(0.366467998634407,1.0561608611351,2.549797875));
#10288=CARTESIAN_POINT('Ctrl Pts',(0.428967998634406,3.12260180609148E-16,
2.549797875));
#10289=CARTESIAN_POINT('Ctrl Pts',(0.491467998634406,-1.0561608611351,2.549797875));
#10290=CARTESIAN_POINT('Ctrl Pts',(0.553967998634406,-1.80297936806755,
1.80297936806755));
#10291=CARTESIAN_POINT('Ctrl Pts',(0.616467998634407,-2.549797875,1.0561608611351));
#10292=CARTESIAN_POINT('Ctrl Pts',(0.678967998634406,-2.549797875,4.68390270913721E-16));
#10293=CARTESIAN_POINT('Ctrl Pts',(0.741467998634407,-2.549797875,-1.0561608611351));
#10294=CARTESIAN_POINT('Ctrl Pts',(0.803967998634406,-1.80297936806755,
-1.80297936806755));
#10295=CARTESIAN_POINT('Ctrl Pts',(0.866467998634405,-1.0561608611351,-2.549797875));
#10296=CARTESIAN_POINT('Ctrl Pts',(0.928967998634406,0.,-2.549797875));
#10297=CARTESIAN_POINT('Ctrl Pts',(-3.75852561669427,0.,-2.00852093905959));
#10298=CARTESIAN_POINT('Ctrl Pts',(-3.69602561669426,0.831956613268825,
-2.00852093905959));
#10299=CARTESIAN_POINT('Ctrl Pts',(-3.63352561669426,1.42023877616421,-1.42023877616421));
#10300=CARTESIAN_POINT('Ctrl Pts',(-3.57102561669426,2.00852093905959,-0.831956613268825));
#10301=CARTESIAN_POINT('Ctrl Pts',(-3.50852561669426,2.00852093905959,-1.22986436951988E-16));
#10302=CARTESIAN_POINT('Ctrl Pts',(-3.44602561669426,2.00852093905959,0.831956613268825));
#10303=CARTESIAN_POINT('Ctrl Pts',(-3.38352561669426,1.42023877616421,1.42023877616421));
#10304=CARTESIAN_POINT('Ctrl Pts',(-3.32102561669426,0.831956613268825,
2.00852093905959));
#10305=CARTESIAN_POINT('Ctrl Pts',(-3.25852561669427,2.45972873903976E-16,
2.00852093905959));
#10306=CARTESIAN_POINT('Ctrl Pts',(-3.19602561669426,-0.831956613268824,
2.00852093905959));
#10307=CARTESIAN_POINT('Ctrl Pts',(-3.13352561669426,-1.42023877616421,
1.42023877616421));
#10308=CARTESIAN_POINT('Ctrl Pts',(-3.07102561669426,-2.00852093905959,
0.831956613268827));
#10309=CARTESIAN_POINT('Ctrl Pts',(-3.00852561669426,-2.00852093905959,
3.68959310855964E-16));
#10310=CARTESIAN_POINT('Ctrl Pts',(-2.94602561669426,-2.00852093905959,
-0.831956613268825));
#10311=CARTESIAN_POINT('Ctrl Pts',(-2.88352561669426,-1.42023877616421,
-1.42023877616421));
#10312=CARTESIAN_POINT('Ctrl Pts',(-2.82102561669426,-0.831956613268827,
-2.00852093905959));
#10313=CARTESIAN_POINT('Ctrl Pts',(-2.75852561669427,0.,-2.00852093905959));
#10314=CARTESIAN_POINT('Ctrl Pts',(-2.69602561669426,0.831956613268825,
-2.00852093905959));
#10315=CARTESIAN_POINT('Ctrl Pts',(-2.63352561669426,1.42023877616421,-1.42023877616421));
#10316=CARTESIAN_POINT('Ctrl Pts',(-2.57102561669426,2.00852093905959,-0.831956613268825));
#10317=CARTESIAN_POINT('Ctrl Pts',(-2.50852561669426,2.00852093905959,-1.22986436951988E-16));
#10318=CARTESIAN_POINT('Ctrl Pts',(-2.44602561669426,2.00852093905959,0.831956613268825));
#10319=CARTESIAN_POINT('Ctrl Pts',(-2.38352561669426,1.42023877616421,1.42023877616421));
#10320=CARTESIAN_POINT('Ctrl Pts',(-2.32102561669426,0.831956613268825,
2.00852093905959));
#10321=CARTESIAN_POINT('Ctrl Pts',(-2.25852561669426,2.45972873903976E-16,
2.00852093905959));
#10322=CARTESIAN_POINT('Ctrl Pts',(-2.19602561669426,-0.831956613268824,
2.00852093905959));
#10323=CARTESIAN_POINT('Ctrl Pts',(-2.13352561669426,-1.42023877616421,
1.42023877616421));
#10324=CARTESIAN_POINT('Ctrl Pts',(-2.07102561669426,-2.00852093905959,
0.831956613268827));
#10325=CARTESIAN_POINT('Ctrl Pts',(-2.00852561669426,-2.00852093905959,
3.68959310855964E-16));
#10326=CARTESIAN_POINT('Ctrl Pts',(-1.94602561669426,-2.00852093905959,
-0.831956613268825));
#10327=CARTESIAN_POINT('Ctrl Pts',(-1.88352561669426,-1.42023877616421,
-1.42023877616421));
#10328=CARTESIAN_POINT('Ctrl Pts',(-1.82102561669426,-0.831956613268827,
-2.00852093905959));
#10329=CARTESIAN_POINT('Ctrl Pts',(-1.75852561669426,0.,-2.00852093905959));
#10330=CARTESIAN_POINT('Ctrl Pts',(-1.69602561669426,0.831956613268825,
-2.00852093905959));
#10331=CARTESIAN_POINT('Ctrl Pts',(-1.63352561669426,1.42023877616421,-1.42023877616421));
#10332=CARTESIAN_POINT('Ctrl Pts',(-1.57102561669426,2.00852093905959,-0.831956613268825));
#10333=CARTESIAN_POINT('Ctrl Pts',(-1.50852561669426,2.00852093905959,-1.22986436951988E-16));
#10334=CARTESIAN_POINT('Ctrl Pts',(-1.44602561669426,2.00852093905959,0.831956613268825));
#10335=CARTESIAN_POINT('Ctrl Pts',(-1.38352561669426,1.42023877616421,1.42023877616421));
#10336=CARTESIAN_POINT('Ctrl Pts',(-1.32102561669426,0.831956613268825,
2.00852093905959));
#10337=CARTESIAN_POINT('Ctrl Pts',(-1.25852561669426,2.45972873903976E-16,
2.00852093905959));
#10338=CARTESIAN_POINT('Ctrl Pts',(-1.19602561669426,-0.831956613268824,
2.00852093905959));
#10339=CARTESIAN_POINT('Ctrl Pts',(-1.13352561669426,-1.42023877616421,
1.42023877616421));
#10340=CARTESIAN_POINT('Ctrl Pts',(-1.07102561669426,-2.00852093905959,
0.831956613268827));
#10341=CARTESIAN_POINT('Ctrl Pts',(-1.00852561669426,-2.00852093905959,
3.68959310855964E-16));
#10342=CARTESIAN_POINT('Ctrl Pts',(-0.946025616694262,-2.00852093905959,
-0.831956613268825));
#10343=CARTESIAN_POINT('Ctrl Pts',(-0.883525616694262,-1.42023877616421,
-1.42023877616421));
#10344=CARTESIAN_POINT('Ctrl Pts',(-0.821025616694261,-0.831956613268827,
-2.00852093905959));
#10345=CARTESIAN_POINT('Ctrl Pts',(-0.758525616694262,0.,-2.00852093905959));
#10346=CARTESIAN_POINT('Ctrl Pts',(-0.696025616694261,0.831956613268825,
-2.00852093905959));
#10347=CARTESIAN_POINT('Ctrl Pts',(-0.633525616694262,1.42023877616421,
-1.42023877616421));
#10348=CARTESIAN_POINT('Ctrl Pts',(-0.571025616694261,2.00852093905959,
-0.831956613268825));
#10349=CARTESIAN_POINT('Ctrl Pts',(-0.508525616694262,2.00852093905959,
-1.22986436951988E-16));
#10350=CARTESIAN_POINT('Ctrl Pts',(-0.446025616694262,2.00852093905959,
0.831956613268825));
#10351=CARTESIAN_POINT('Ctrl Pts',(-0.383525616694262,1.42023877616421,
1.42023877616421));
#10352=CARTESIAN_POINT('Ctrl Pts',(-0.321025616694262,0.831956613268825,
2.00852093905959));
#10353=CARTESIAN_POINT('Ctrl Pts',(-0.258525616694262,2.45972873903976E-16,
2.00852093905959));
#10354=CARTESIAN_POINT('Ctrl Pts',(-0.196025616694262,-0.831956613268824,
2.00852093905959));
#10355=CARTESIAN_POINT('Ctrl Pts',(-0.133525616694262,-1.42023877616421,
1.42023877616421));
#10356=CARTESIAN_POINT('Ctrl Pts',(-0.0710256166942618,-2.00852093905959,
0.831956613268827));
#10357=CARTESIAN_POINT('Ctrl Pts',(-0.00852561669426215,-2.00852093905959,
3.68959310855964E-16));
#10358=CARTESIAN_POINT('Ctrl Pts',(0.0539743833057379,-2.00852093905959,
-0.831956613268825));
#10359=CARTESIAN_POINT('Ctrl Pts',(0.116474383305738,-1.42023877616421,
-1.42023877616421));
#10360=CARTESIAN_POINT('Ctrl Pts',(0.178974383305738,-0.831956613268827,
-2.00852093905959));
#10361=CARTESIAN_POINT('Ctrl Pts',(0.241474383305738,0.,-2.00852093905959));
#10362=CARTESIAN_POINT('Ctrl Pts',(0.303974383305738,0.831956613268825,
-2.00852093905959));
#10363=CARTESIAN_POINT('Ctrl Pts',(0.366474383305738,1.42023877616421,-1.42023877616421));
#10364=CARTESIAN_POINT('Ctrl Pts',(0.428974383305738,2.00852093905959,-0.831956613268825));
#10365=CARTESIAN_POINT('Ctrl Pts',(0.491474383305738,2.00852093905959,-1.22986436951988E-16));
#10366=CARTESIAN_POINT('Ctrl Pts',(0.553974383305738,2.00852093905959,0.831956613268825));
#10367=CARTESIAN_POINT('Ctrl Pts',(0.616474383305739,1.42023877616421,1.42023877616421));
#10368=CARTESIAN_POINT('Ctrl Pts',(0.678974383305738,0.831956613268825,
2.00852093905959));
#10369=CARTESIAN_POINT('Ctrl Pts',(0.741474383305739,2.45972873903976E-16,
2.00852093905959));
#10370=CARTESIAN_POINT('Ctrl Pts',(0.803974383305737,-0.831956613268824,
2.00852093905959));
#10371=CARTESIAN_POINT('Ctrl Pts',(0.866474383305738,-1.42023877616421,
1.42023877616421));
#10372=CARTESIAN_POINT('Ctrl Pts',(0.928974383305737,-2.00852093905959,
0.831956613268827));
#10373=CARTESIAN_POINT('Ctrl Pts',(0.991474383305738,-2.00852093905959,
3.68959310855964E-16));
#10374=CARTESIAN_POINT('Ctrl Pts',(1.05397438330574,-2.00852093905959,-0.831956613268825));
#10375=CARTESIAN_POINT('Ctrl Pts',(1.11647438330574,-1.42023877616421,-1.42023877616421));
#10376=CARTESIAN_POINT('Ctrl Pts',(1.17897438330574,-0.831956613268827,
-2.00852093905959));
#10377=CARTESIAN_POINT('Ctrl Pts',(1.24147438330574,0.,-2.00852093905959));
#10378=CARTESIAN_POINT('',(16.7581062602089,-31.2052008701535,10.2199939419596));
#10379=CARTESIAN_POINT('',(45.7581062602089,-6.20520087015334,22.2199939419596));
#10380=CARTESIAN_POINT('',(45.7581062602089,-6.20520087015377,15.2199939419596));
#10381=CARTESIAN_POINT('',(45.7581062602089,8.7947991298465,24.2199939419596));
#10382=CARTESIAN_POINT('',(45.7581062602089,-6.20520087015379,27.2199939419596));
#10383=CARTESIAN_POINT('',(45.8753511262408,-6.17380127923249,-4.78000605804049));
#10384=CARTESIAN_POINT('',(45.7581062602089,-6.20520087015373,-10.0300060580404));
#10385=CARTESIAN_POINT('',(60.7581062602088,-6.2052008701534,6.21999394195957));
#10386=CARTESIAN_POINT('',(45.7581062602089,-6.20520087015366,6.21999394195957));
#10387=CARTESIAN_POINT('',(45.7581062602089,-6.20520087015377,8.21999394195957));
#10388=CARTESIAN_POINT('',(30.7581062602089,-6.2052008701534,24.2199939419596));
#10389=CARTESIAN_POINT('',(45.7581062602089,-21.2052008701535,24.2199939419596));
#10390=CARTESIAN_POINT('',(60.7581062602089,-6.20520087015318,24.2199939419596));
#10391=CARTESIAN_POINT('',(45.7581062602089,-21.2052008701535,6.21999394195957));
#10392=CARTESIAN_POINT('',(30.7581062602088,-6.2052008701535,6.21999394195957));
#10393=CARTESIAN_POINT('',(45.7581062602089,8.7947991298465,6.21999394195957));
#10394=UNCERTAINTY_MEASURE_WITH_UNIT(LENGTH_MEASURE(0.01),#10414,
'DISTANCE_ACCURACY_VALUE',
'Maximum model space distance between geometric entities at asserted c
onnectivities');
#10395=UNCERTAINTY_MEASURE_WITH_UNIT(LENGTH_MEASURE(0.01),#10414,
'DISTANCE_ACCURACY_VALUE',
'Maximum model space distance between geometric entities at asserted c
onnectivities');
#10396=UNCERTAINTY_MEASURE_WITH_UNIT(LENGTH_MEASURE(0.01),#10414,
'DISTANCE_ACCURACY_VALUE',
'Maximum model space distance between geometric entities at asserted c
onnectivities');
#10397=UNCERTAINTY_MEASURE_WITH_UNIT(LENGTH_MEASURE(0.01),#10414,
'DISTANCE_ACCURACY_VALUE',
'Maximum model space distance between geometric entities at asserted c
onnectivities');
#10398=UNCERTAINTY_MEASURE_WITH_UNIT(LENGTH_MEASURE(0.01),#10414,
'DISTANCE_ACCURACY_VALUE',
'Maximum model space distance between geometric entities at asserted c
onnectivities');
#10399=UNCERTAINTY_MEASURE_WITH_UNIT(LENGTH_MEASURE(0.01),#10414,
'DISTANCE_ACCURACY_VALUE',
'Maximum model space distance between geometric entities at asserted c
onnectivities');
#10400=UNCERTAINTY_MEASURE_WITH_UNIT(LENGTH_MEASURE(0.01),#10414,
'DISTANCE_ACCURACY_VALUE',
'Maximum model space distance between geometric entities at asserted c
onnectivities');
#10401=UNCERTAINTY_MEASURE_WITH_UNIT(LENGTH_MEASURE(0.01),#10414,
'DISTANCE_ACCURACY_VALUE',
'Maximum model space distance between geometric entities at asserted c
onnectivities');
#10402=UNCERTAINTY_MEASURE_WITH_UNIT(LENGTH_MEASURE(0.01),#10414,
'DISTANCE_ACCURACY_VALUE',
'Maximum model space distance between geometric entities at asserted c
onnectivities');
#10403=UNCERTAINTY_MEASURE_WITH_UNIT(LENGTH_MEASURE(0.01),#10414,
'DISTANCE_ACCURACY_VALUE',
'Maximum model space distance between geometric entities at asserted c
onnectivities');
#10404=(
GEOMETRIC_REPRESENTATION_CONTEXT(3)
GLOBAL_UNCERTAINTY_ASSIGNED_CONTEXT((#10394))
GLOBAL_UNIT_ASSIGNED_CONTEXT((#10414,#10416,#10417))
REPRESENTATION_CONTEXT('','3D')
);
#10405=(
GEOMETRIC_REPRESENTATION_CONTEXT(3)
GLOBAL_UNCERTAINTY_ASSIGNED_CONTEXT((#10395))
GLOBAL_UNIT_ASSIGNED_CONTEXT((#10414,#10416,#10417))
REPRESENTATION_CONTEXT('','3D')
);
#10406=(
GEOMETRIC_REPRESENTATION_CONTEXT(3)
GLOBAL_UNCERTAINTY_ASSIGNED_CONTEXT((#10396))
GLOBAL_UNIT_ASSIGNED_CONTEXT((#10414,#10416,#10417))
REPRESENTATION_CONTEXT('','3D')
);
#10407=(
GEOMETRIC_REPRESENTATION_CONTEXT(3)
GLOBAL_UNCERTAINTY_ASSIGNED_CONTEXT((#10397))
GLOBAL_UNIT_ASSIGNED_CONTEXT((#10414,#10416,#10417))
REPRESENTATION_CONTEXT('','3D')
);
#10408=(
GEOMETRIC_REPRESENTATION_CONTEXT(3)
GLOBAL_UNCERTAINTY_ASSIGNED_CONTEXT((#10398))
GLOBAL_UNIT_ASSIGNED_CONTEXT((#10414,#10416,#10417))
REPRESENTATION_CONTEXT('','3D')
);
#10409=(
GEOMETRIC_REPRESENTATION_CONTEXT(3)
GLOBAL_UNCERTAINTY_ASSIGNED_CONTEXT((#10399))
GLOBAL_UNIT_ASSIGNED_CONTEXT((#10414,#10416,#10417))
REPRESENTATION_CONTEXT('','3D')
);
#10410=(
GEOMETRIC_REPRESENTATION_CONTEXT(3)
GLOBAL_UNCERTAINTY_ASSIGNED_CONTEXT((#10400))
GLOBAL_UNIT_ASSIGNED_CONTEXT((#10414,#10416,#10417))
REPRESENTATION_CONTEXT('','3D')
);
#10411=(
GEOMETRIC_REPRESENTATION_CONTEXT(3)
GLOBAL_UNCERTAINTY_ASSIGNED_CONTEXT((#10401))
GLOBAL_UNIT_ASSIGNED_CONTEXT((#10414,#10416,#10417))
REPRESENTATION_CONTEXT('','3D')
);
#10412=(
GEOMETRIC_REPRESENTATION_CONTEXT(3)
GLOBAL_UNCERTAINTY_ASSIGNED_CONTEXT((#10402))
GLOBAL_UNIT_ASSIGNED_CONTEXT((#10414,#10416,#10417))
REPRESENTATION_CONTEXT('','3D')
);
#10413=(
GEOMETRIC_REPRESENTATION_CONTEXT(3)
GLOBAL_UNCERTAINTY_ASSIGNED_CONTEXT((#10403))
GLOBAL_UNIT_ASSIGNED_CONTEXT((#10414,#10416,#10417))
REPRESENTATION_CONTEXT('','3D')
);
#10414=(
LENGTH_UNIT()
NAMED_UNIT(*)
SI_UNIT(.MILLI.,.METRE.)
);
#10415=(
LENGTH_UNIT()
NAMED_UNIT(*)
SI_UNIT($,.METRE.)
);
#10416=(
NAMED_UNIT(*)
PLANE_ANGLE_UNIT()
SI_UNIT($,.RADIAN.)
);
#10417=(
NAMED_UNIT(*)
SI_UNIT($,.STERADIAN.)
SOLID_ANGLE_UNIT()
);
#10418=SHAPE_DEFINITION_REPRESENTATION(#10427,#10452);
#10419=SHAPE_DEFINITION_REPRESENTATION(#10428,#10453);
#10420=SHAPE_DEFINITION_REPRESENTATION(#10429,#10454);
#10421=SHAPE_DEFINITION_REPRESENTATION(#10430,#10455);
#10422=SHAPE_DEFINITION_REPRESENTATION(#10431,#10456);
#10423=SHAPE_DEFINITION_REPRESENTATION(#10432,#10457);
#10424=SHAPE_DEFINITION_REPRESENTATION(#10433,#10458);
#10425=SHAPE_DEFINITION_REPRESENTATION(#10434,#10459);
#10426=SHAPE_DEFINITION_REPRESENTATION(#10435,#10460);
#10427=PRODUCT_DEFINITION_SHAPE('',$,#10462);
#10428=PRODUCT_DEFINITION_SHAPE('',$,#10463);
#10429=PRODUCT_DEFINITION_SHAPE('',$,#10464);
#10430=PRODUCT_DEFINITION_SHAPE('',$,#10465);
#10431=PRODUCT_DEFINITION_SHAPE('',$,#10466);
#10432=PRODUCT_DEFINITION_SHAPE('',$,#10467);
#10433=PRODUCT_DEFINITION_SHAPE('',$,#10468);
#10434=PRODUCT_DEFINITION_SHAPE('',$,#10469);
#10435=PRODUCT_DEFINITION_SHAPE('',$,#10470);
#10436=PRODUCT_DEFINITION_SHAPE($,$,#59);
#10437=PRODUCT_DEFINITION_SHAPE($,$,#60);
#10438=PRODUCT_DEFINITION_SHAPE($,$,#61);
#10439=PRODUCT_DEFINITION_SHAPE($,$,#62);
#10440=PRODUCT_DEFINITION_SHAPE($,$,#63);
#10441=PRODUCT_DEFINITION_SHAPE($,$,#64);
#10442=PRODUCT_DEFINITION_SHAPE($,$,#65);
#10443=PRODUCT_DEFINITION_SHAPE($,$,#66);
#10444=PRODUCT_DEFINITION_SHAPE($,$,#67);
#10445=PRODUCT_DEFINITION_SHAPE($,$,#68);
#10446=PRODUCT_DEFINITION_SHAPE($,$,#69);
#10447=PRODUCT_DEFINITION_SHAPE($,$,#70);
#10448=PRODUCT_DEFINITION_SHAPE($,$,#71);
#10449=PRODUCT_DEFINITION_SHAPE($,$,#72);
#10450=PRODUCT_DEFINITION_SHAPE($,$,#73);
#10451=PRODUCT_DEFINITION_SHAPE($,$,#74);
#10452=SHAPE_REPRESENTATION('',(#5396,#6134,#6135,#6136,#6137,#6138,#6139,
#6140,#6141,#6142,#6143,#6144,#6145,#6146,#6147,#6148,#6149),#10404);
#10453=SHAPE_REPRESENTATION('',(#5397),#10405);
#10454=SHAPE_REPRESENTATION('',(#5435),#10406);
#10455=SHAPE_REPRESENTATION('',(#5466),#10407);
#10456=SHAPE_REPRESENTATION('',(#6015),#10408);
#10457=SHAPE_REPRESENTATION('',(#6051),#10409);
#10458=SHAPE_REPRESENTATION('',(#6076),#10410);
#10459=SHAPE_REPRESENTATION('',(#6085),#10411);
#10460=SHAPE_REPRESENTATION('',(#6098),#10412);
#10461=PRODUCT_DEFINITION_CONTEXT('part definition',#10490,'design');
#10462=PRODUCT_DEFINITION('MAT-016','MAT-016',#10471,#10461);
#10463=PRODUCT_DEFINITION('Angle Bracket','Angle Bracket',#10472,#10461);
#10464=PRODUCT_DEFINITION('Shaft','Shaft',#10473,#10461);
#10465=PRODUCT_DEFINITION('Spur Gear','Spur Gear',#10474,#10461);
#10466=PRODUCT_DEFINITION('Hex nut M8','Hex Nut M8',#10475,#10461);
#10467=PRODUCT_DEFINITION('Disc Plate','Disc Plate',#10476,#10461);
#10468=PRODUCT_DEFINITION('Spacer','Spacer',#10477,#10461);
#10469=PRODUCT_DEFINITION('Hex Bolt','Hex Bolt',#10478,#10461);
#10470=PRODUCT_DEFINITION('Hex Nut M5','Hex Nut M5',#10479,#10461);
#10471=PRODUCT_DEFINITION_FORMATION('',$,#10492);
#10472=PRODUCT_DEFINITION_FORMATION('',$,#10493);
#10473=PRODUCT_DEFINITION_FORMATION('',$,#10494);
#10474=PRODUCT_DEFINITION_FORMATION('',$,#10495);
#10475=PRODUCT_DEFINITION_FORMATION('',$,#10496);
#10476=PRODUCT_DEFINITION_FORMATION('',$,#10497);
#10477=PRODUCT_DEFINITION_FORMATION('',$,#10498);
#10478=PRODUCT_DEFINITION_FORMATION('',$,#10499);
#10479=PRODUCT_DEFINITION_FORMATION('',$,#10500);
#10480=PRODUCT_RELATED_PRODUCT_CATEGORY('MAT-016','MAT-016',(#10492));
#10481=PRODUCT_RELATED_PRODUCT_CATEGORY('Angle Bracket','Angle Bracket',
(#10493));
#10482=PRODUCT_RELATED_PRODUCT_CATEGORY('Shaft','Shaft',(#10494));
#10483=PRODUCT_RELATED_PRODUCT_CATEGORY('Spur Gear','Spur Gear',(#10495));
#10484=PRODUCT_RELATED_PRODUCT_CATEGORY('Hex Nut M8','Hex Nut M8',(#10496));
#10485=PRODUCT_RELATED_PRODUCT_CATEGORY('Disc Plate','Disc Plate',(#10497));
#10486=PRODUCT_RELATED_PRODUCT_CATEGORY('Spacer','Spacer',(#10498));
#10487=PRODUCT_RELATED_PRODUCT_CATEGORY('Hex Bolt','Hex Bolt',(#10499));
#10488=PRODUCT_RELATED_PRODUCT_CATEGORY('Hex Nut M5','Hex Nut M5',(#10500));
#10489=APPLICATION_PROTOCOL_DEFINITION('international standard',
'automotive_design',2009,#10490);
#10490=APPLICATION_CONTEXT(
'Core Data for Automotive Mechanical Design Process');
#10491=PRODUCT_CONTEXT('part definition',#10490,'mechanical');
#10492=PRODUCT('MAT-016','MAT-016','STEP AP214',(#10491));
#10493=PRODUCT('Angle Bracket','Angle Bracket',$,(#10491));
#10494=PRODUCT('Shaft','Shaft','Shaft',(#10491));
#10495=PRODUCT('Spur Gear','Spur Gear',$,(#10491));
#10496=PRODUCT('Hex nut M8','Hex Nut M8',$,(#10491));
#10497=PRODUCT('Disc Plate','Disc Plate',$,(#10491));
#10498=PRODUCT('Spacer','Spacer',$,(#10491));
#10499=PRODUCT('Hex Bolt','Hex Bolt',$,(#10491));
#10500=PRODUCT('Hex Nut M5','Hex Nut M5',$,(#10491));
#10501=PRESENTATION_STYLE_ASSIGNMENT((#10505));
#10502=PRESENTATION_STYLE_ASSIGNMENT((#10506));
#10503=PRESENTATION_STYLE_ASSIGNMENT((#10507));
#10504=PRESENTATION_STYLE_ASSIGNMENT((#10508));
#10505=SURFACE_STYLE_USAGE(.BOTH.,#10509);
#10506=SURFACE_STYLE_USAGE(.BOTH.,#10510);
#10507=SURFACE_STYLE_USAGE(.BOTH.,#10511);
#10508=SURFACE_STYLE_USAGE(.BOTH.,#10512);
#10509=SURFACE_SIDE_STYLE('',(#10513));
#10510=SURFACE_SIDE_STYLE('',(#10514));
#10511=SURFACE_SIDE_STYLE('',(#10515));
#10512=SURFACE_SIDE_STYLE('',(#10516));
#10513=SURFACE_STYLE_FILL_AREA(#10517);
#10514=SURFACE_STYLE_FILL_AREA(#10518);
#10515=SURFACE_STYLE_FILL_AREA(#10519);
#10516=SURFACE_STYLE_FILL_AREA(#10520);
#10517=FILL_AREA_STYLE('Steel - Satin',(#10521));
#10518=FILL_AREA_STYLE('Opaque(61,176,222)',(#10522));
#10519=FILL_AREA_STYLE('Opaque(97,158,199)',(#10523));
#10520=FILL_AREA_STYLE('Opaque(227,224,212)',(#10524));
#10521=FILL_AREA_STYLE_COLOUR('Steel - Satin',#10525);
#10522=FILL_AREA_STYLE_COLOUR('Opaque(61,176,222)',#10526);
#10523=FILL_AREA_STYLE_COLOUR('Opaque(97,158,199)',#10527);
#10524=FILL_AREA_STYLE_COLOUR('Opaque(227,224,212)',#10528);
#10525=COLOUR_RGB('Steel - Satin',0.627450980392157,0.627450980392157,0.627450980392157);
#10526=COLOUR_RGB('Opaque(61,176,222)',0.23921568627451,0.690196078431373,
0.870588235294118);
#10527=COLOUR_RGB('Opaque(97,158,199)',0.380392156862745,0.619607843137255,
0.780392156862745);
#10528=COLOUR_RGB('Opaque(227,224,212)',0.890196078431372,0.87843137254902,
0.831372549019608);
ENDSEC;
END-ISO-10303-21;
